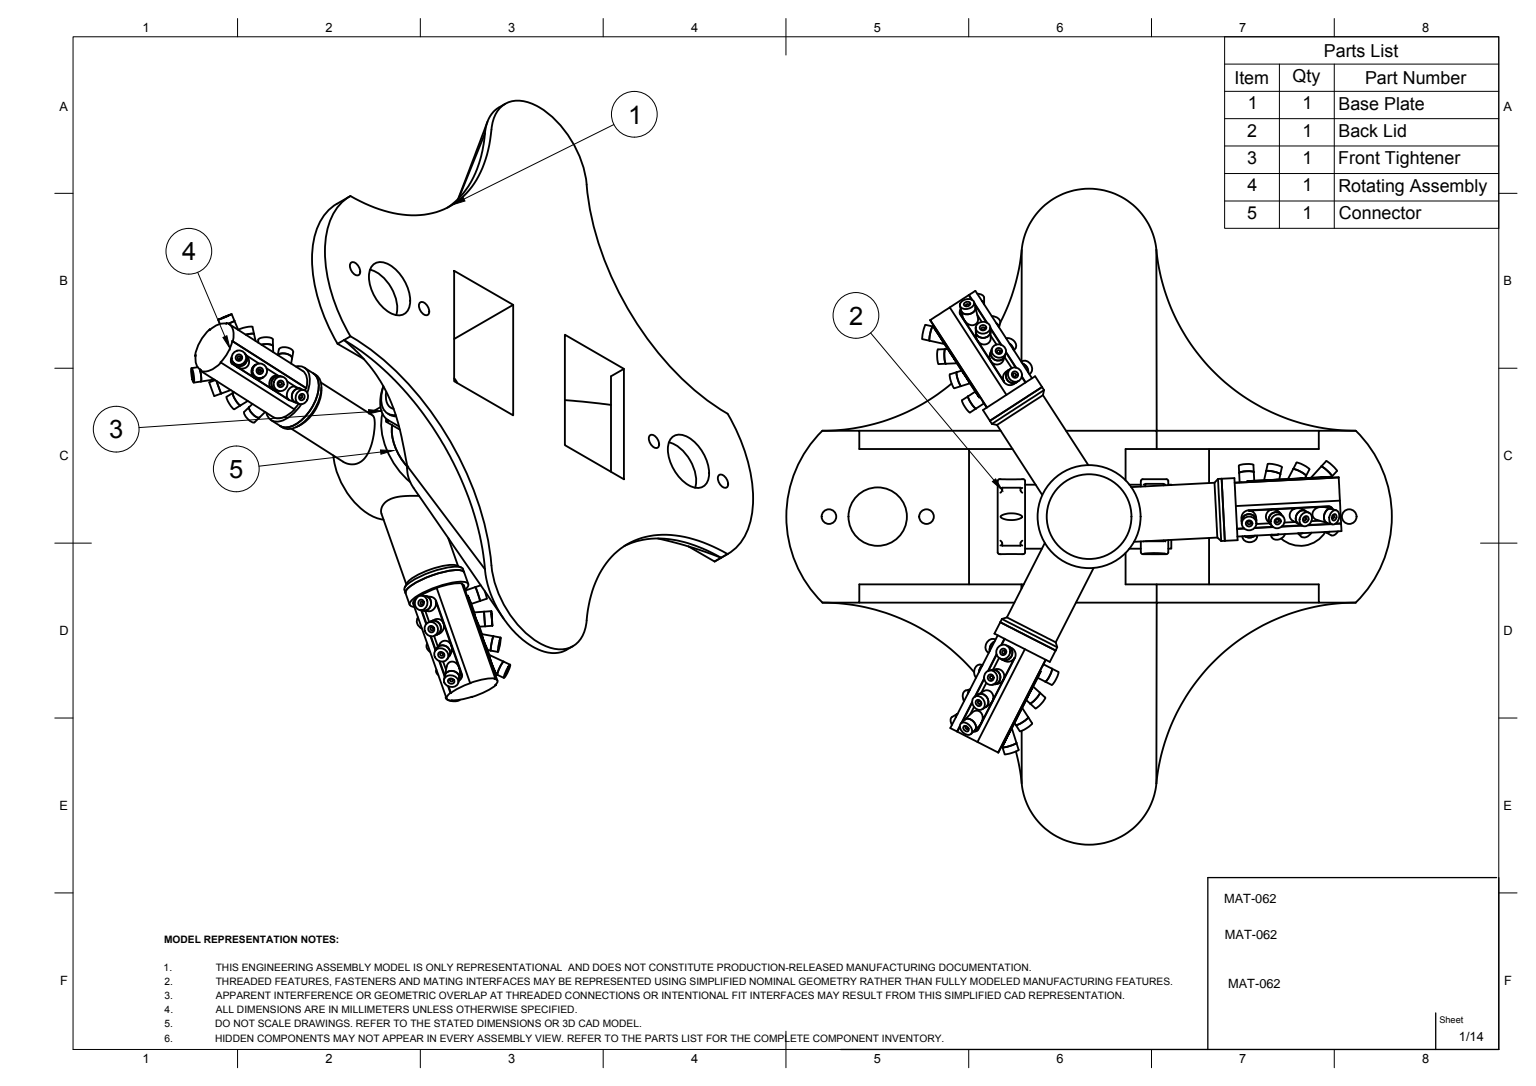
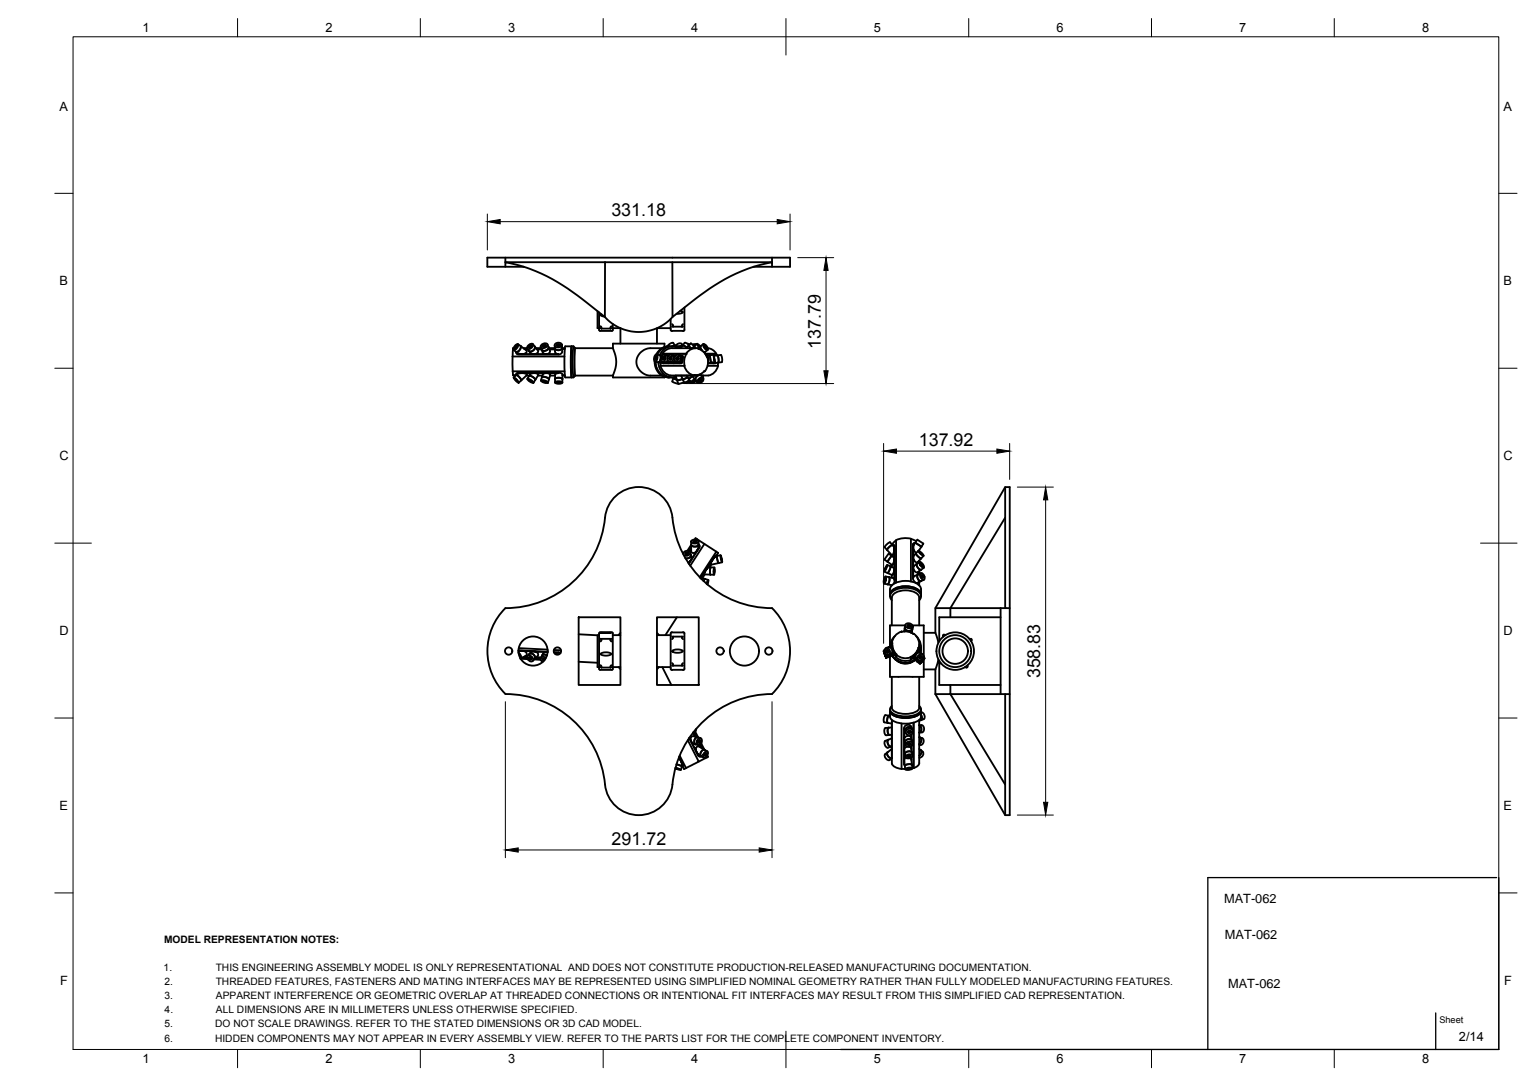
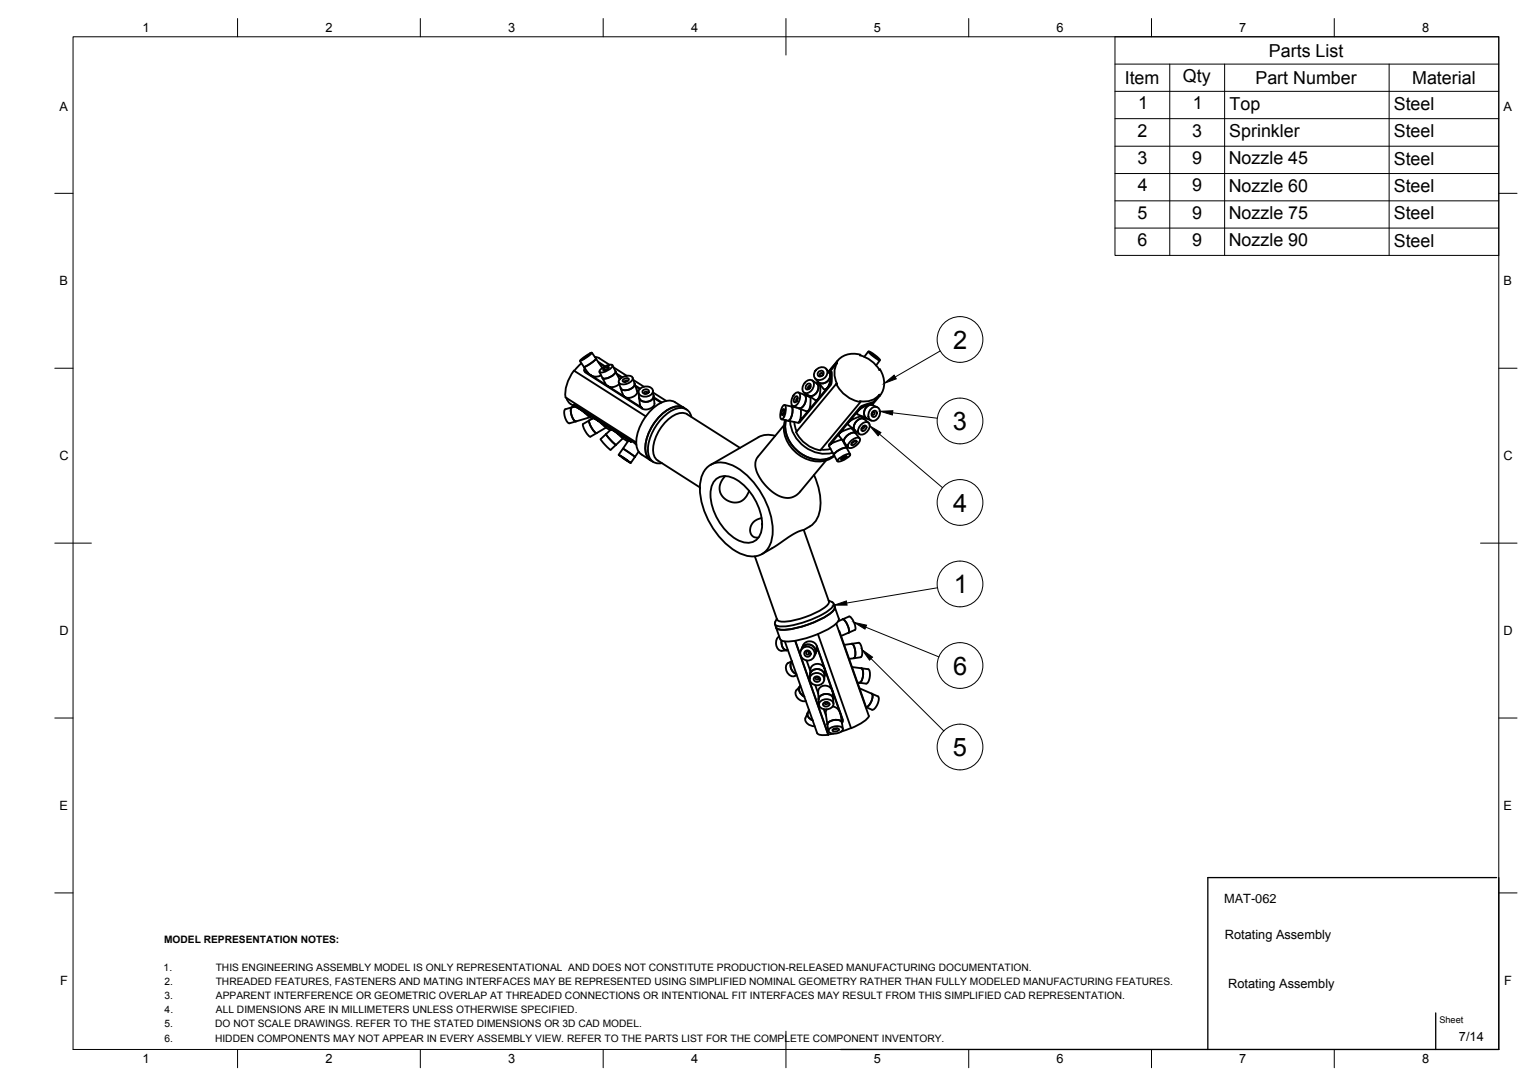
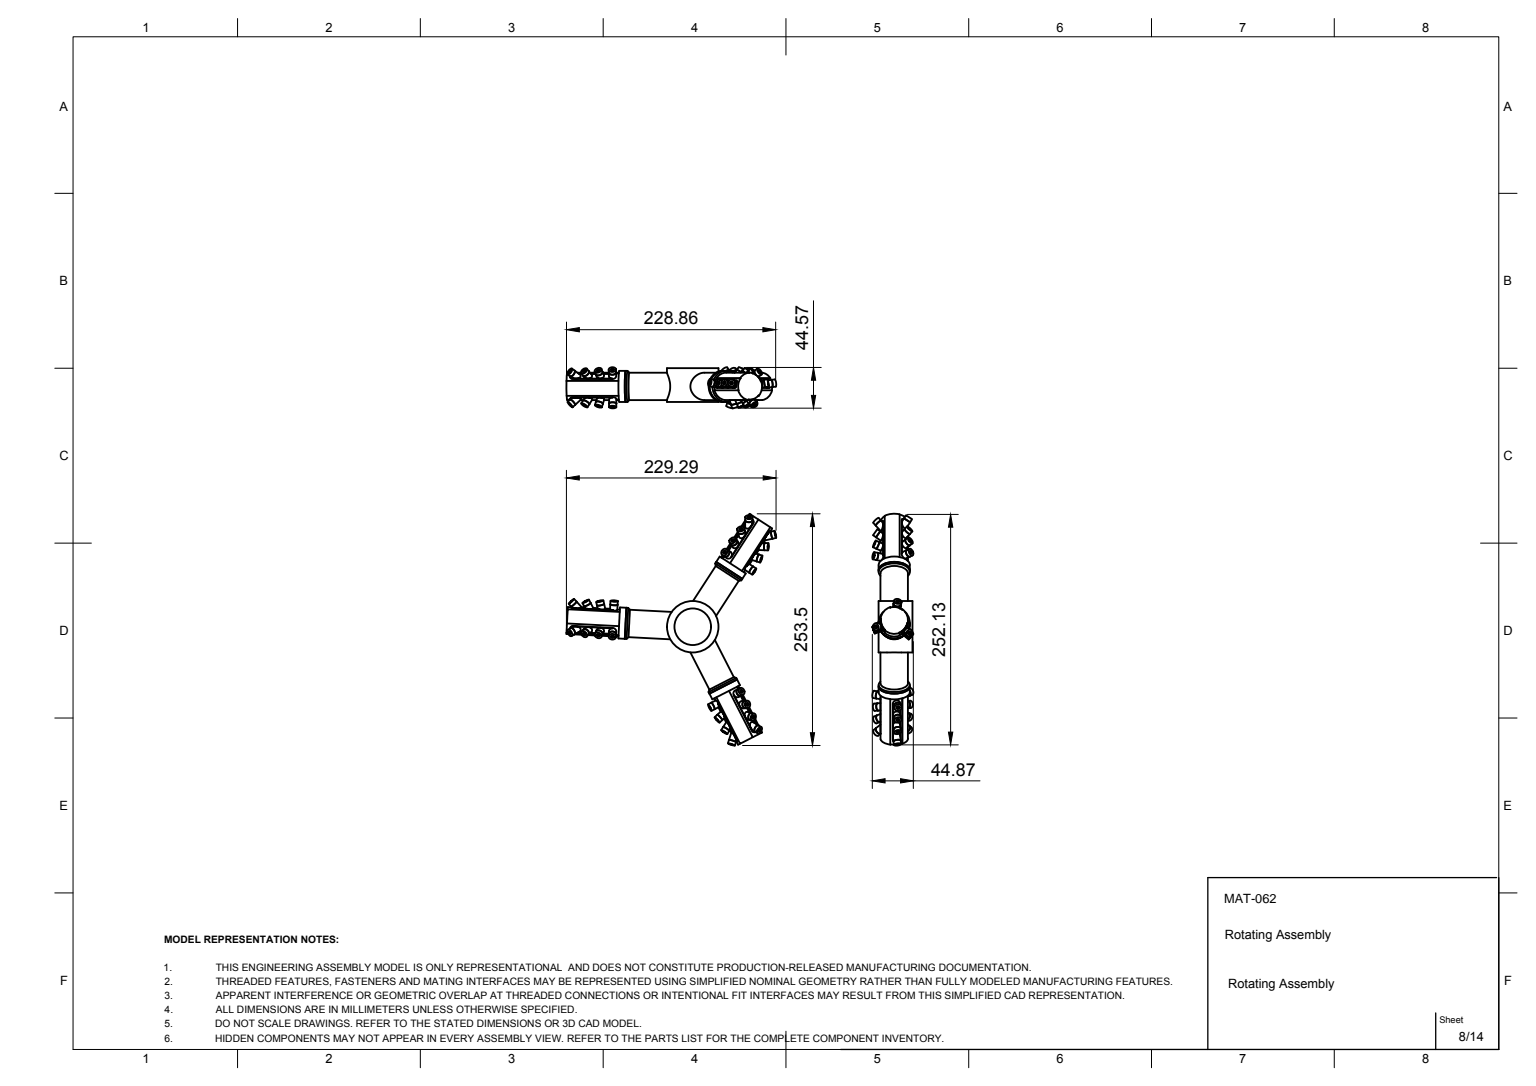
ISO-10303-21;
HEADER;
/* Generated by software containing ST-Developer
 * from STEP Tools, Inc. (www.steptools.com) 
 */

FILE_DESCRIPTION(
/* description */ (''),
/* implementation_level */ '2;1');

FILE_NAME(
/* name */ 'MAT-062',
/* time_stamp */ '2026-10-24T10:18:25-07:00',
/* author */ (''),
/* organization */ (''),
/* preprocessor_version */ 'ST-DEVELOPER v20.2',
/* originating_system */ 'Autodesk Translation Framework v15.15.0.0',
/* authorisation */ '');

FILE_SCHEMA (('AUTOMOTIVE_DESIGN { 1 0 10303 214 3 1 1 }'));
ENDSEC;

DATA;
#10=MECHANICAL_DESIGN_GEOMETRIC_PRESENTATION_REPRESENTATION('',(#247,#248,
#249,#250,#251,#252,#253,#254,#255,#256,#257,#258,#259,#260,#261,#262,#263,
#264,#265),#14125);
#11=ITEM_DEFINED_TRANSFORMATION($,$,#6478,#6849);
#12=ITEM_DEFINED_TRANSFORMATION($,$,#6669,#6850);
#13=ITEM_DEFINED_TRANSFORMATION($,$,#6624,#6851);
#14=ITEM_DEFINED_TRANSFORMATION($,$,#6609,#6852);
#15=ITEM_DEFINED_TRANSFORMATION($,$,#6639,#6853);
#16=ITEM_DEFINED_TRANSFORMATION($,$,#6654,#6854);
#17=ITEM_DEFINED_TRANSFORMATION($,$,#6624,#6855);
#18=ITEM_DEFINED_TRANSFORMATION($,$,#6624,#6856);
#19=ITEM_DEFINED_TRANSFORMATION($,$,#6609,#6857);
#20=ITEM_DEFINED_TRANSFORMATION($,$,#6609,#6858);
#21=ITEM_DEFINED_TRANSFORMATION($,$,#6639,#6859);
#22=ITEM_DEFINED_TRANSFORMATION($,$,#6639,#6860);
#23=ITEM_DEFINED_TRANSFORMATION($,$,#6654,#6861);
#24=ITEM_DEFINED_TRANSFORMATION($,$,#6654,#6862);
#25=ITEM_DEFINED_TRANSFORMATION($,$,#6654,#6863);
#26=ITEM_DEFINED_TRANSFORMATION($,$,#6654,#6864);
#27=ITEM_DEFINED_TRANSFORMATION($,$,#6639,#6865);
#28=ITEM_DEFINED_TRANSFORMATION($,$,#6639,#6866);
#29=ITEM_DEFINED_TRANSFORMATION($,$,#6609,#6867);
#30=ITEM_DEFINED_TRANSFORMATION($,$,#6609,#6868);
#31=ITEM_DEFINED_TRANSFORMATION($,$,#6624,#6869);
#32=ITEM_DEFINED_TRANSFORMATION($,$,#6624,#6870);
#33=ITEM_DEFINED_TRANSFORMATION($,$,#6609,#6871);
#34=ITEM_DEFINED_TRANSFORMATION($,$,#6609,#6872);
#35=ITEM_DEFINED_TRANSFORMATION($,$,#6624,#6873);
#36=ITEM_DEFINED_TRANSFORMATION($,$,#6624,#6874);
#37=ITEM_DEFINED_TRANSFORMATION($,$,#6639,#6875);
#38=ITEM_DEFINED_TRANSFORMATION($,$,#6639,#6876);
#39=ITEM_DEFINED_TRANSFORMATION($,$,#6654,#6877);
#40=ITEM_DEFINED_TRANSFORMATION($,$,#6654,#6878);
#41=ITEM_DEFINED_TRANSFORMATION($,$,#6609,#6879);
#42=ITEM_DEFINED_TRANSFORMATION($,$,#6609,#6880);
#43=ITEM_DEFINED_TRANSFORMATION($,$,#6624,#6881);
#44=ITEM_DEFINED_TRANSFORMATION($,$,#6624,#6882);
#45=ITEM_DEFINED_TRANSFORMATION($,$,#6639,#6883);
#46=ITEM_DEFINED_TRANSFORMATION($,$,#6639,#6884);
#47=ITEM_DEFINED_TRANSFORMATION($,$,#6654,#6885);
#48=ITEM_DEFINED_TRANSFORMATION($,$,#6654,#6886);
#49=ITEM_DEFINED_TRANSFORMATION($,$,#6669,#6887);
#50=ITEM_DEFINED_TRANSFORMATION($,$,#6669,#6888);
#51=ITEM_DEFINED_TRANSFORMATION($,$,#6259,#6902);
#52=ITEM_DEFINED_TRANSFORMATION($,$,#6338,#6903);
#53=ITEM_DEFINED_TRANSFORMATION($,$,#6408,#6904);
#54=ITEM_DEFINED_TRANSFORMATION($,$,#6477,#6905);
#55=ITEM_DEFINED_TRANSFORMATION($,$,#6889,#6906);
#56=(
REPRESENTATION_RELATIONSHIP($,$,#14204,#14203)
REPRESENTATION_RELATIONSHIP_WITH_TRANSFORMATION(#11)
SHAPE_REPRESENTATION_RELATIONSHIP()
);
#57=(
REPRESENTATION_RELATIONSHIP($,$,#14209,#14203)
REPRESENTATION_RELATIONSHIP_WITH_TRANSFORMATION(#12)
SHAPE_REPRESENTATION_RELATIONSHIP()
);
#58=(
REPRESENTATION_RELATIONSHIP($,$,#14206,#14203)
REPRESENTATION_RELATIONSHIP_WITH_TRANSFORMATION(#13)
SHAPE_REPRESENTATION_RELATIONSHIP()
);
#59=(
REPRESENTATION_RELATIONSHIP($,$,#14205,#14203)
REPRESENTATION_RELATIONSHIP_WITH_TRANSFORMATION(#14)
SHAPE_REPRESENTATION_RELATIONSHIP()
);
#60=(
REPRESENTATION_RELATIONSHIP($,$,#14207,#14203)
REPRESENTATION_RELATIONSHIP_WITH_TRANSFORMATION(#15)
SHAPE_REPRESENTATION_RELATIONSHIP()
);
#61=(
REPRESENTATION_RELATIONSHIP($,$,#14208,#14203)
REPRESENTATION_RELATIONSHIP_WITH_TRANSFORMATION(#16)
SHAPE_REPRESENTATION_RELATIONSHIP()
);
#62=(
REPRESENTATION_RELATIONSHIP($,$,#14206,#14203)
REPRESENTATION_RELATIONSHIP_WITH_TRANSFORMATION(#17)
SHAPE_REPRESENTATION_RELATIONSHIP()
);
#63=(
REPRESENTATION_RELATIONSHIP($,$,#14206,#14203)
REPRESENTATION_RELATIONSHIP_WITH_TRANSFORMATION(#18)
SHAPE_REPRESENTATION_RELATIONSHIP()
);
#64=(
REPRESENTATION_RELATIONSHIP($,$,#14205,#14203)
REPRESENTATION_RELATIONSHIP_WITH_TRANSFORMATION(#19)
SHAPE_REPRESENTATION_RELATIONSHIP()
);
#65=(
REPRESENTATION_RELATIONSHIP($,$,#14205,#14203)
REPRESENTATION_RELATIONSHIP_WITH_TRANSFORMATION(#20)
SHAPE_REPRESENTATION_RELATIONSHIP()
);
#66=(
REPRESENTATION_RELATIONSHIP($,$,#14207,#14203)
REPRESENTATION_RELATIONSHIP_WITH_TRANSFORMATION(#21)
SHAPE_REPRESENTATION_RELATIONSHIP()
);
#67=(
REPRESENTATION_RELATIONSHIP($,$,#14207,#14203)
REPRESENTATION_RELATIONSHIP_WITH_TRANSFORMATION(#22)
SHAPE_REPRESENTATION_RELATIONSHIP()
);
#68=(
REPRESENTATION_RELATIONSHIP($,$,#14208,#14203)
REPRESENTATION_RELATIONSHIP_WITH_TRANSFORMATION(#23)
SHAPE_REPRESENTATION_RELATIONSHIP()
);
#69=(
REPRESENTATION_RELATIONSHIP($,$,#14208,#14203)
REPRESENTATION_RELATIONSHIP_WITH_TRANSFORMATION(#24)
SHAPE_REPRESENTATION_RELATIONSHIP()
);
#70=(
REPRESENTATION_RELATIONSHIP($,$,#14208,#14203)
REPRESENTATION_RELATIONSHIP_WITH_TRANSFORMATION(#25)
SHAPE_REPRESENTATION_RELATIONSHIP()
);
#71=(
REPRESENTATION_RELATIONSHIP($,$,#14208,#14203)
REPRESENTATION_RELATIONSHIP_WITH_TRANSFORMATION(#26)
SHAPE_REPRESENTATION_RELATIONSHIP()
);
#72=(
REPRESENTATION_RELATIONSHIP($,$,#14207,#14203)
REPRESENTATION_RELATIONSHIP_WITH_TRANSFORMATION(#27)
SHAPE_REPRESENTATION_RELATIONSHIP()
);
#73=(
REPRESENTATION_RELATIONSHIP($,$,#14207,#14203)
REPRESENTATION_RELATIONSHIP_WITH_TRANSFORMATION(#28)
SHAPE_REPRESENTATION_RELATIONSHIP()
);
#74=(
REPRESENTATION_RELATIONSHIP($,$,#14205,#14203)
REPRESENTATION_RELATIONSHIP_WITH_TRANSFORMATION(#29)
SHAPE_REPRESENTATION_RELATIONSHIP()
);
#75=(
REPRESENTATION_RELATIONSHIP($,$,#14205,#14203)
REPRESENTATION_RELATIONSHIP_WITH_TRANSFORMATION(#30)
SHAPE_REPRESENTATION_RELATIONSHIP()
);
#76=(
REPRESENTATION_RELATIONSHIP($,$,#14206,#14203)
REPRESENTATION_RELATIONSHIP_WITH_TRANSFORMATION(#31)
SHAPE_REPRESENTATION_RELATIONSHIP()
);
#77=(
REPRESENTATION_RELATIONSHIP($,$,#14206,#14203)
REPRESENTATION_RELATIONSHIP_WITH_TRANSFORMATION(#32)
SHAPE_REPRESENTATION_RELATIONSHIP()
);
#78=(
REPRESENTATION_RELATIONSHIP($,$,#14205,#14203)
REPRESENTATION_RELATIONSHIP_WITH_TRANSFORMATION(#33)
SHAPE_REPRESENTATION_RELATIONSHIP()
);
#79=(
REPRESENTATION_RELATIONSHIP($,$,#14205,#14203)
REPRESENTATION_RELATIONSHIP_WITH_TRANSFORMATION(#34)
SHAPE_REPRESENTATION_RELATIONSHIP()
);
#80=(
REPRESENTATION_RELATIONSHIP($,$,#14206,#14203)
REPRESENTATION_RELATIONSHIP_WITH_TRANSFORMATION(#35)
SHAPE_REPRESENTATION_RELATIONSHIP()
);
#81=(
REPRESENTATION_RELATIONSHIP($,$,#14206,#14203)
REPRESENTATION_RELATIONSHIP_WITH_TRANSFORMATION(#36)
SHAPE_REPRESENTATION_RELATIONSHIP()
);
#82=(
REPRESENTATION_RELATIONSHIP($,$,#14207,#14203)
REPRESENTATION_RELATIONSHIP_WITH_TRANSFORMATION(#37)
SHAPE_REPRESENTATION_RELATIONSHIP()
);
#83=(
REPRESENTATION_RELATIONSHIP($,$,#14207,#14203)
REPRESENTATION_RELATIONSHIP_WITH_TRANSFORMATION(#38)
SHAPE_REPRESENTATION_RELATIONSHIP()
);
#84=(
REPRESENTATION_RELATIONSHIP($,$,#14208,#14203)
REPRESENTATION_RELATIONSHIP_WITH_TRANSFORMATION(#39)
SHAPE_REPRESENTATION_RELATIONSHIP()
);
#85=(
REPRESENTATION_RELATIONSHIP($,$,#14208,#14203)
REPRESENTATION_RELATIONSHIP_WITH_TRANSFORMATION(#40)
SHAPE_REPRESENTATION_RELATIONSHIP()
);
#86=(
REPRESENTATION_RELATIONSHIP($,$,#14205,#14203)
REPRESENTATION_RELATIONSHIP_WITH_TRANSFORMATION(#41)
SHAPE_REPRESENTATION_RELATIONSHIP()
);
#87=(
REPRESENTATION_RELATIONSHIP($,$,#14205,#14203)
REPRESENTATION_RELATIONSHIP_WITH_TRANSFORMATION(#42)
SHAPE_REPRESENTATION_RELATIONSHIP()
);
#88=(
REPRESENTATION_RELATIONSHIP($,$,#14206,#14203)
REPRESENTATION_RELATIONSHIP_WITH_TRANSFORMATION(#43)
SHAPE_REPRESENTATION_RELATIONSHIP()
);
#89=(
REPRESENTATION_RELATIONSHIP($,$,#14206,#14203)
REPRESENTATION_RELATIONSHIP_WITH_TRANSFORMATION(#44)
SHAPE_REPRESENTATION_RELATIONSHIP()
);
#90=(
REPRESENTATION_RELATIONSHIP($,$,#14207,#14203)
REPRESENTATION_RELATIONSHIP_WITH_TRANSFORMATION(#45)
SHAPE_REPRESENTATION_RELATIONSHIP()
);
#91=(
REPRESENTATION_RELATIONSHIP($,$,#14207,#14203)
REPRESENTATION_RELATIONSHIP_WITH_TRANSFORMATION(#46)
SHAPE_REPRESENTATION_RELATIONSHIP()
);
#92=(
REPRESENTATION_RELATIONSHIP($,$,#14208,#14203)
REPRESENTATION_RELATIONSHIP_WITH_TRANSFORMATION(#47)
SHAPE_REPRESENTATION_RELATIONSHIP()
);
#93=(
REPRESENTATION_RELATIONSHIP($,$,#14208,#14203)
REPRESENTATION_RELATIONSHIP_WITH_TRANSFORMATION(#48)
SHAPE_REPRESENTATION_RELATIONSHIP()
);
#94=(
REPRESENTATION_RELATIONSHIP($,$,#14209,#14203)
REPRESENTATION_RELATIONSHIP_WITH_TRANSFORMATION(#49)
SHAPE_REPRESENTATION_RELATIONSHIP()
);
#95=(
REPRESENTATION_RELATIONSHIP($,$,#14209,#14203)
REPRESENTATION_RELATIONSHIP_WITH_TRANSFORMATION(#50)
SHAPE_REPRESENTATION_RELATIONSHIP()
);
#96=(
REPRESENTATION_RELATIONSHIP($,$,#14200,#14199)
REPRESENTATION_RELATIONSHIP_WITH_TRANSFORMATION(#51)
SHAPE_REPRESENTATION_RELATIONSHIP()
);
#97=(
REPRESENTATION_RELATIONSHIP($,$,#14201,#14199)
REPRESENTATION_RELATIONSHIP_WITH_TRANSFORMATION(#52)
SHAPE_REPRESENTATION_RELATIONSHIP()
);
#98=(
REPRESENTATION_RELATIONSHIP($,$,#14202,#14199)
REPRESENTATION_RELATIONSHIP_WITH_TRANSFORMATION(#53)
SHAPE_REPRESENTATION_RELATIONSHIP()
);
#99=(
REPRESENTATION_RELATIONSHIP($,$,#14203,#14199)
REPRESENTATION_RELATIONSHIP_WITH_TRANSFORMATION(#54)
SHAPE_REPRESENTATION_RELATIONSHIP()
);
#100=(
REPRESENTATION_RELATIONSHIP($,$,#14210,#14199)
REPRESENTATION_RELATIONSHIP_WITH_TRANSFORMATION(#55)
SHAPE_REPRESENTATION_RELATIONSHIP()
);
#101=CONTEXT_DEPENDENT_SHAPE_REPRESENTATION(#56,#14153);
#102=CONTEXT_DEPENDENT_SHAPE_REPRESENTATION(#57,#14154);
#103=CONTEXT_DEPENDENT_SHAPE_REPRESENTATION(#58,#14155);
#104=CONTEXT_DEPENDENT_SHAPE_REPRESENTATION(#59,#14156);
#105=CONTEXT_DEPENDENT_SHAPE_REPRESENTATION(#60,#14157);
#106=CONTEXT_DEPENDENT_SHAPE_REPRESENTATION(#61,#14158);
#107=CONTEXT_DEPENDENT_SHAPE_REPRESENTATION(#62,#14159);
#108=CONTEXT_DEPENDENT_SHAPE_REPRESENTATION(#63,#14160);
#109=CONTEXT_DEPENDENT_SHAPE_REPRESENTATION(#64,#14161);
#110=CONTEXT_DEPENDENT_SHAPE_REPRESENTATION(#65,#14162);
#111=CONTEXT_DEPENDENT_SHAPE_REPRESENTATION(#66,#14163);
#112=CONTEXT_DEPENDENT_SHAPE_REPRESENTATION(#67,#14164);
#113=CONTEXT_DEPENDENT_SHAPE_REPRESENTATION(#68,#14165);
#114=CONTEXT_DEPENDENT_SHAPE_REPRESENTATION(#69,#14166);
#115=CONTEXT_DEPENDENT_SHAPE_REPRESENTATION(#70,#14167);
#116=CONTEXT_DEPENDENT_SHAPE_REPRESENTATION(#71,#14168);
#117=CONTEXT_DEPENDENT_SHAPE_REPRESENTATION(#72,#14169);
#118=CONTEXT_DEPENDENT_SHAPE_REPRESENTATION(#73,#14170);
#119=CONTEXT_DEPENDENT_SHAPE_REPRESENTATION(#74,#14171);
#120=CONTEXT_DEPENDENT_SHAPE_REPRESENTATION(#75,#14172);
#121=CONTEXT_DEPENDENT_SHAPE_REPRESENTATION(#76,#14173);
#122=CONTEXT_DEPENDENT_SHAPE_REPRESENTATION(#77,#14174);
#123=CONTEXT_DEPENDENT_SHAPE_REPRESENTATION(#78,#14175);
#124=CONTEXT_DEPENDENT_SHAPE_REPRESENTATION(#79,#14176);
#125=CONTEXT_DEPENDENT_SHAPE_REPRESENTATION(#80,#14177);
#126=CONTEXT_DEPENDENT_SHAPE_REPRESENTATION(#81,#14178);
#127=CONTEXT_DEPENDENT_SHAPE_REPRESENTATION(#82,#14179);
#128=CONTEXT_DEPENDENT_SHAPE_REPRESENTATION(#83,#14180);
#129=CONTEXT_DEPENDENT_SHAPE_REPRESENTATION(#84,#14181);
#130=CONTEXT_DEPENDENT_SHAPE_REPRESENTATION(#85,#14182);
#131=CONTEXT_DEPENDENT_SHAPE_REPRESENTATION(#86,#14183);
#132=CONTEXT_DEPENDENT_SHAPE_REPRESENTATION(#87,#14184);
#133=CONTEXT_DEPENDENT_SHAPE_REPRESENTATION(#88,#14185);
#134=CONTEXT_DEPENDENT_SHAPE_REPRESENTATION(#89,#14186);
#135=CONTEXT_DEPENDENT_SHAPE_REPRESENTATION(#90,#14187);
#136=CONTEXT_DEPENDENT_SHAPE_REPRESENTATION(#91,#14188);
#137=CONTEXT_DEPENDENT_SHAPE_REPRESENTATION(#92,#14189);
#138=CONTEXT_DEPENDENT_SHAPE_REPRESENTATION(#93,#14190);
#139=CONTEXT_DEPENDENT_SHAPE_REPRESENTATION(#94,#14191);
#140=CONTEXT_DEPENDENT_SHAPE_REPRESENTATION(#95,#14192);
#141=CONTEXT_DEPENDENT_SHAPE_REPRESENTATION(#96,#14194);
#142=CONTEXT_DEPENDENT_SHAPE_REPRESENTATION(#97,#14195);
#143=CONTEXT_DEPENDENT_SHAPE_REPRESENTATION(#98,#14196);
#144=CONTEXT_DEPENDENT_SHAPE_REPRESENTATION(#99,#14197);
#145=CONTEXT_DEPENDENT_SHAPE_REPRESENTATION(#100,#14198);
#146=NEXT_ASSEMBLY_USAGE_OCCURRENCE('Top:1','Top:1','Top:1',#14216,#14217,
'Top:1');
#147=NEXT_ASSEMBLY_USAGE_OCCURRENCE('Sprinkler:1','Sprinkler:1',
'Sprinkler:1',#14216,#14222,'Sprinkler:1');
#148=NEXT_ASSEMBLY_USAGE_OCCURRENCE('Nozzle 45:1','Nozzle 45:1',
'Nozzle 45:1',#14216,#14219,'Nozzle 45:1');
#149=NEXT_ASSEMBLY_USAGE_OCCURRENCE('Nozzle 60:1','Nozzle 60:1',
'Nozzle 60:1',#14216,#14218,'Nozzle 60:1');
#150=NEXT_ASSEMBLY_USAGE_OCCURRENCE('Nozzle 75:1','Nozzle 75:1',
'Nozzle 75:1',#14216,#14220,'Nozzle 75:1');
#151=NEXT_ASSEMBLY_USAGE_OCCURRENCE('Nozzle 90:1','Nozzle 90:1',
'Nozzle 90:1',#14216,#14221,'Nozzle 90:1');
#152=NEXT_ASSEMBLY_USAGE_OCCURRENCE('Nozzle 45:2','Nozzle 45:2',
'Nozzle 45:2',#14216,#14219,'Nozzle 45:2');
#153=NEXT_ASSEMBLY_USAGE_OCCURRENCE('Nozzle 45:3','Nozzle 45:3',
'Nozzle 45:3',#14216,#14219,'Nozzle 45:3');
#154=NEXT_ASSEMBLY_USAGE_OCCURRENCE('Nozzle 60:2','Nozzle 60:2',
'Nozzle 60:2',#14216,#14218,'Nozzle 60:2');
#155=NEXT_ASSEMBLY_USAGE_OCCURRENCE('Nozzle 60:3','Nozzle 60:3',
'Nozzle 60:3',#14216,#14218,'Nozzle 60:3');
#156=NEXT_ASSEMBLY_USAGE_OCCURRENCE('Nozzle 75:2','Nozzle 75:2',
'Nozzle 75:2',#14216,#14220,'Nozzle 75:2');
#157=NEXT_ASSEMBLY_USAGE_OCCURRENCE('Nozzle 75:3','Nozzle 75:3',
'Nozzle 75:3',#14216,#14220,'Nozzle 75:3');
#158=NEXT_ASSEMBLY_USAGE_OCCURRENCE('Nozzle 90:2','Nozzle 90:2',
'Nozzle 90:2',#14216,#14221,'Nozzle 90:2');
#159=NEXT_ASSEMBLY_USAGE_OCCURRENCE('Nozzle 90:3','Nozzle 90:3',
'Nozzle 90:3',#14216,#14221,'Nozzle 90:3');
#160=NEXT_ASSEMBLY_USAGE_OCCURRENCE('Nozzle 90:4','Nozzle 90:4',
'Nozzle 90:4',#14216,#14221,'Nozzle 90:4');
#161=NEXT_ASSEMBLY_USAGE_OCCURRENCE('Nozzle 90:5','Nozzle 90:5',
'Nozzle 90:5',#14216,#14221,'Nozzle 90:5');
#162=NEXT_ASSEMBLY_USAGE_OCCURRENCE('Nozzle 75:4','Nozzle 75:4',
'Nozzle 75:4',#14216,#14220,'Nozzle 75:4');
#163=NEXT_ASSEMBLY_USAGE_OCCURRENCE('Nozzle 75:5','Nozzle 75:5',
'Nozzle 75:5',#14216,#14220,'Nozzle 75:5');
#164=NEXT_ASSEMBLY_USAGE_OCCURRENCE('Nozzle 60:4','Nozzle 60:4',
'Nozzle 60:4',#14216,#14218,'Nozzle 60:4');
#165=NEXT_ASSEMBLY_USAGE_OCCURRENCE('Nozzle 60:5','Nozzle 60:5',
'Nozzle 60:5',#14216,#14218,'Nozzle 60:5');
#166=NEXT_ASSEMBLY_USAGE_OCCURRENCE('Nozzle 45:4','Nozzle 45:4',
'Nozzle 45:4',#14216,#14219,'Nozzle 45:4');
#167=NEXT_ASSEMBLY_USAGE_OCCURRENCE('Nozzle 45:5','Nozzle 45:5',
'Nozzle 45:5',#14216,#14219,'Nozzle 45:5');
#168=NEXT_ASSEMBLY_USAGE_OCCURRENCE('Nozzle 60:6','Nozzle 60:6',
'Nozzle 60:6',#14216,#14218,'Nozzle 60:6');
#169=NEXT_ASSEMBLY_USAGE_OCCURRENCE('Nozzle 60:7','Nozzle 60:7',
'Nozzle 60:7',#14216,#14218,'Nozzle 60:7');
#170=NEXT_ASSEMBLY_USAGE_OCCURRENCE('Nozzle 45:6','Nozzle 45:6',
'Nozzle 45:6',#14216,#14219,'Nozzle 45:6');
#171=NEXT_ASSEMBLY_USAGE_OCCURRENCE('Nozzle 45:7','Nozzle 45:7',
'Nozzle 45:7',#14216,#14219,'Nozzle 45:7');
#172=NEXT_ASSEMBLY_USAGE_OCCURRENCE('Nozzle 75:6','Nozzle 75:6',
'Nozzle 75:6',#14216,#14220,'Nozzle 75:6');
#173=NEXT_ASSEMBLY_USAGE_OCCURRENCE('Nozzle 75:7','Nozzle 75:7',
'Nozzle 75:7',#14216,#14220,'Nozzle 75:7');
#174=NEXT_ASSEMBLY_USAGE_OCCURRENCE('Nozzle 90:6','Nozzle 90:6',
'Nozzle 90:6',#14216,#14221,'Nozzle 90:6');
#175=NEXT_ASSEMBLY_USAGE_OCCURRENCE('Nozzle 90:7','Nozzle 90:7',
'Nozzle 90:7',#14216,#14221,'Nozzle 90:7');
#176=NEXT_ASSEMBLY_USAGE_OCCURRENCE('Nozzle 60:8','Nozzle 60:8',
'Nozzle 60:8',#14216,#14218,'Nozzle 60:8');
#177=NEXT_ASSEMBLY_USAGE_OCCURRENCE('Nozzle 60:9','Nozzle 60:9',
'Nozzle 60:9',#14216,#14218,'Nozzle 60:9');
#178=NEXT_ASSEMBLY_USAGE_OCCURRENCE('Nozzle 45:8','Nozzle 45:8',
'Nozzle 45:8',#14216,#14219,'Nozzle 45:8');
#179=NEXT_ASSEMBLY_USAGE_OCCURRENCE('Nozzle 45:9','Nozzle 45:9',
'Nozzle 45:9',#14216,#14219,'Nozzle 45:9');
#180=NEXT_ASSEMBLY_USAGE_OCCURRENCE('Nozzle 75:8','Nozzle 75:8',
'Nozzle 75:8',#14216,#14220,'Nozzle 75:8');
#181=NEXT_ASSEMBLY_USAGE_OCCURRENCE('Nozzle 75:9','Nozzle 75:9',
'Nozzle 75:9',#14216,#14220,'Nozzle 75:9');
#182=NEXT_ASSEMBLY_USAGE_OCCURRENCE('Nozzle 90:8','Nozzle 90:8',
'Nozzle 90:8',#14216,#14221,'Nozzle 90:8');
#183=NEXT_ASSEMBLY_USAGE_OCCURRENCE('Nozzle 90:9','Nozzle 90:9',
'Nozzle 90:9',#14216,#14221,'Nozzle 90:9');
#184=NEXT_ASSEMBLY_USAGE_OCCURRENCE('Sprinkler:2','Sprinkler:2',
'Sprinkler:2',#14216,#14222,'Sprinkler:2');
#185=NEXT_ASSEMBLY_USAGE_OCCURRENCE('Sprinkler:3','Sprinkler:3',
'Sprinkler:3',#14216,#14222,'Sprinkler:3');
#186=NEXT_ASSEMBLY_USAGE_OCCURRENCE('Base Plate:1','Base Plate:1',
'Base Plate:1',#14212,#14213,'Base Plate:1');
#187=NEXT_ASSEMBLY_USAGE_OCCURRENCE('Back Lid:1','Back Lid:1',
'Back Lid:1',#14212,#14214,'Back Lid:1');
#188=NEXT_ASSEMBLY_USAGE_OCCURRENCE('Front Tightener:1',
'Front Tightener:1','Front Tightener:1',#14212,#14215,
'Front Tightener:1');
#189=NEXT_ASSEMBLY_USAGE_OCCURRENCE('Rotating Assembly:1',
'Rotating Assembly:1','Rotating Assembly:1',#14212,#14216,
'Rotating Assembly:1');
#190=NEXT_ASSEMBLY_USAGE_OCCURRENCE('Connector:1','Connector:1',
'Connector:1',#14212,#14223,'Connector:1');
#191=CONICAL_SURFACE('',#6560,17.,0.785398163397448);
#192=CONICAL_SURFACE('',#6577,17.,0.785398163397452);
#193=CONICAL_SURFACE('',#6578,17.,0.785398163397448);
#194=CONICAL_SURFACE('',#6620,1.8,0.785398163397439);
#195=CONICAL_SURFACE('',#6635,1.8,0.785398163397447);
#196=CONICAL_SURFACE('',#6650,1.80000000000001,0.785398163397454);
#197=CONICAL_SURFACE('',#6665,1.8,0.785398163397448);
#198=CONICAL_SURFACE('',#6890,16.,0.0349065850398866);
#199=TOROIDAL_SURFACE('',#6365,21.5,1.);
#200=TOROIDAL_SURFACE('',#6366,21.5,1.);
#201=TOROIDAL_SURFACE('',#6390,21.5,1.);
#202=TOROIDAL_SURFACE('',#6391,21.5,1.);
#203=TOROIDAL_SURFACE('',#6394,21.5,1.);
#204=TOROIDAL_SURFACE('',#6395,21.5,1.);
#205=TOROIDAL_SURFACE('',#6398,21.5,1.);
#206=TOROIDAL_SURFACE('',#6399,21.5,1.);
#207=TOROIDAL_SURFACE('',#6401,19.5,1.);
#208=TOROIDAL_SURFACE('',#6403,19.5,1.);
#209=TOROIDAL_SURFACE('',#6436,21.5,1.);
#210=TOROIDAL_SURFACE('',#6437,21.5,1.);
#211=TOROIDAL_SURFACE('',#6461,21.5,1.);
#212=TOROIDAL_SURFACE('',#6462,21.5,1.);
#213=TOROIDAL_SURFACE('',#6465,21.5,1.);
#214=TOROIDAL_SURFACE('',#6466,21.5,1.);
#215=TOROIDAL_SURFACE('',#6469,21.5,1.);
#216=TOROIDAL_SURFACE('',#6470,21.5,1.);
#217=TOROIDAL_SURFACE('',#6472,19.5,1.);
#218=TOROIDAL_SURFACE('',#6474,19.5,1.);
#219=(
BOUNDED_SURFACE()
B_SPLINE_SURFACE(2,2,((#10435,#10436,#10437,#10438,#10439),(#10440,#10441,
#10442,#10443,#10444),(#10445,#10446,#10447,#10448,#10449)),
 .UNSPECIFIED.,.F.,.F.,.F.)
B_SPLINE_SURFACE_WITH_KNOTS((3,3),(3,2,3),(-0.372145961557786,0.372122372471418),
(-2.5862005619648,-1.57539112175776,-0.564581681550713),.UNSPECIFIED.)
GEOMETRIC_REPRESENTATION_ITEM()
RATIONAL_B_SPLINE_SURFACE(((1.,0.874978596158143,1.,0.874978596158143,1.),
(0.931553475244656,0.815089352015808,0.931553475244656,0.815089352015808,
0.931553475244656),(1.,0.874978596158143,1.,0.874978596158143,1.)))
REPRESENTATION_ITEM('')
SURFACE()
);
#220=(
BOUNDED_SURFACE()
B_SPLINE_SURFACE(2,2,((#10450,#10451,#10452,#10453,#10454),(#10455,#10456,
#10457,#10458,#10459),(#10460,#10461,#10462,#10463,#10464)),
 .UNSPECIFIED.,.F.,.F.,.F.)
B_SPLINE_SURFACE_WITH_KNOTS((3,3),(3,2,3),(-0.372145961557785,0.372122372471416),
(-1.01540423516984,-0.00459479496282911,1.00621464524418),.UNSPECIFIED.)
GEOMETRIC_REPRESENTATION_ITEM()
RATIONAL_B_SPLINE_SURFACE(((1.,0.874978596158151,1.,0.874978596158151,1.),
(0.931553475244656,0.815089352015816,0.931553475244656,0.815089352015816,
0.931553475244656),(1.,0.874978596158151,1.,0.874978596158151,1.)))
REPRESENTATION_ITEM('')
SURFACE()
);
#221=(
BOUNDED_SURFACE()
B_SPLINE_SURFACE(2,2,((#10465,#10466,#10467,#10468,#10469),(#10470,#10471,
#10472,#10473,#10474),(#10475,#10476,#10477,#10478,#10479)),
 .UNSPECIFIED.,.F.,.F.,.F.)
B_SPLINE_SURFACE_WITH_KNOTS((3,3),(3,2,3),(-0.372145961557786,0.372122372471418),
(0.555392091624955,1.56620153183202,2.57701097203908),.UNSPECIFIED.)
GEOMETRIC_REPRESENTATION_ITEM()
RATIONAL_B_SPLINE_SURFACE(((1.,0.874978596158138,1.,0.874978596158138,1.),
(0.931553475244654,0.815089352015803,0.931553475244654,0.815089352015803,
0.931553475244654),(1.,0.874978596158138,1.,0.874978596158138,1.)))
REPRESENTATION_ITEM('')
SURFACE()
);
#222=(
BOUNDED_SURFACE()
B_SPLINE_SURFACE(2,2,((#10480,#10481,#10482,#10483,#10484),(#10485,#10486,
#10487,#10488,#10489),(#10490,#10491,#10492,#10493,#10494)),
 .UNSPECIFIED.,.F.,.F.,.F.)
B_SPLINE_SURFACE_WITH_KNOTS((3,3),(3,2,3),(-0.371934671474245,0.371934671474244),
(-1.01080944020701,0.,1.01080944020701),.UNSPECIFIED.)
GEOMETRIC_REPRESENTATION_ITEM()
RATIONAL_B_SPLINE_SURFACE(((1.,0.87497859615815,1.,0.87497859615815,1.),
(0.93162599415309,0.815152804508512,0.93162599415309,0.815152804508512,
0.93162599415309),(1.,0.87497859615815,1.,0.87497859615815,1.)))
REPRESENTATION_ITEM('')
SURFACE()
);
#223=(
BOUNDED_SURFACE()
B_SPLINE_SURFACE(2,2,((#11091,#11092,#11093,#11094,#11095),(#11096,#11097,
#11098,#11099,#11100),(#11101,#11102,#11103,#11104,#11105)),
 .UNSPECIFIED.,.F.,.F.,.F.)
B_SPLINE_SURFACE_WITH_KNOTS((3,3),(3,2,3),(-0.372145961557786,0.372122372471418),
(-2.5862005619648,-1.57539112175776,-0.564581681550713),.UNSPECIFIED.)
GEOMETRIC_REPRESENTATION_ITEM()
RATIONAL_B_SPLINE_SURFACE(((1.,0.874978596158143,1.,0.874978596158143,1.),
(0.931553475244656,0.815089352015808,0.931553475244656,0.815089352015808,
0.931553475244656),(1.,0.874978596158143,1.,0.874978596158143,1.)))
REPRESENTATION_ITEM('')
SURFACE()
);
#224=(
BOUNDED_SURFACE()
B_SPLINE_SURFACE(2,2,((#11106,#11107,#11108,#11109,#11110),(#11111,#11112,
#11113,#11114,#11115),(#11116,#11117,#11118,#11119,#11120)),
 .UNSPECIFIED.,.F.,.F.,.F.)
B_SPLINE_SURFACE_WITH_KNOTS((3,3),(3,2,3),(-0.372145961557785,0.372122372471416),
(-1.01540423516984,-0.00459479496282911,1.00621464524418),.UNSPECIFIED.)
GEOMETRIC_REPRESENTATION_ITEM()
RATIONAL_B_SPLINE_SURFACE(((1.,0.874978596158151,1.,0.874978596158151,1.),
(0.931553475244656,0.815089352015816,0.931553475244656,0.815089352015816,
0.931553475244656),(1.,0.874978596158151,1.,0.874978596158151,1.)))
REPRESENTATION_ITEM('')
SURFACE()
);
#225=(
BOUNDED_SURFACE()
B_SPLINE_SURFACE(2,2,((#11121,#11122,#11123,#11124,#11125),(#11126,#11127,
#11128,#11129,#11130),(#11131,#11132,#11133,#11134,#11135)),
 .UNSPECIFIED.,.F.,.F.,.F.)
B_SPLINE_SURFACE_WITH_KNOTS((3,3),(3,2,3),(-0.372145961557786,0.372122372471418),
(0.555392091624955,1.56620153183202,2.57701097203908),.UNSPECIFIED.)
GEOMETRIC_REPRESENTATION_ITEM()
RATIONAL_B_SPLINE_SURFACE(((1.,0.874978596158138,1.,0.874978596158138,1.),
(0.931553475244654,0.815089352015803,0.931553475244654,0.815089352015803,
0.931553475244654),(1.,0.874978596158138,1.,0.874978596158138,1.)))
REPRESENTATION_ITEM('')
SURFACE()
);
#226=(
BOUNDED_SURFACE()
B_SPLINE_SURFACE(2,2,((#11136,#11137,#11138,#11139,#11140),(#11141,#11142,
#11143,#11144,#11145),(#11146,#11147,#11148,#11149,#11150)),
 .UNSPECIFIED.,.F.,.F.,.F.)
B_SPLINE_SURFACE_WITH_KNOTS((3,3),(3,2,3),(-0.371934671474245,0.371934671474244),
(-1.01080944020701,0.,1.01080944020701),.UNSPECIFIED.)
GEOMETRIC_REPRESENTATION_ITEM()
RATIONAL_B_SPLINE_SURFACE(((1.,0.87497859615815,1.,0.87497859615815,1.),
(0.93162599415309,0.815152804508512,0.93162599415309,0.815152804508512,
0.93162599415309),(1.,0.87497859615815,1.,0.87497859615815,1.)))
REPRESENTATION_ITEM('')
SURFACE()
);
#227=SHAPE_REPRESENTATION_RELATIONSHIP('SRR','None',#14200,#237);
#228=SHAPE_REPRESENTATION_RELATIONSHIP('SRR','None',#14201,#238);
#229=SHAPE_REPRESENTATION_RELATIONSHIP('SRR','None',#14202,#239);
#230=SHAPE_REPRESENTATION_RELATIONSHIP('SRR','None',#14204,#240);
#231=SHAPE_REPRESENTATION_RELATIONSHIP('SRR','None',#14205,#241);
#232=SHAPE_REPRESENTATION_RELATIONSHIP('SRR','None',#14206,#242);
#233=SHAPE_REPRESENTATION_RELATIONSHIP('SRR','None',#14207,#243);
#234=SHAPE_REPRESENTATION_RELATIONSHIP('SRR','None',#14208,#244);
#235=SHAPE_REPRESENTATION_RELATIONSHIP('SRR','None',#14209,#245);
#236=SHAPE_REPRESENTATION_RELATIONSHIP('SRR','None',#14210,#246);
#237=ADVANCED_BREP_SHAPE_REPRESENTATION('',(#266),#14114);
#238=ADVANCED_BREP_SHAPE_REPRESENTATION('',(#267),#14115);
#239=ADVANCED_BREP_SHAPE_REPRESENTATION('',(#268),#14116);
#240=ADVANCED_BREP_SHAPE_REPRESENTATION('',(#269,#270,#271,#272),#14118);
#241=ADVANCED_BREP_SHAPE_REPRESENTATION('',(#273),#14119);
#242=ADVANCED_BREP_SHAPE_REPRESENTATION('',(#274),#14120);
#243=ADVANCED_BREP_SHAPE_REPRESENTATION('',(#275),#14121);
#244=ADVANCED_BREP_SHAPE_REPRESENTATION('',(#276),#14122);
#245=ADVANCED_BREP_SHAPE_REPRESENTATION('',(#277),#14123);
#246=ADVANCED_BREP_SHAPE_REPRESENTATION('',(#278),#14124);
#247=STYLED_ITEM('',(#14263),#266);
#248=STYLED_ITEM('',(#14263),#267);
#249=STYLED_ITEM('',(#14263),#268);
#250=STYLED_ITEM('',(#14263),#269);
#251=STYLED_ITEM('',(#14263),#270);
#252=STYLED_ITEM('',(#14263),#271);
#253=STYLED_ITEM('',(#14264),#5964);
#254=STYLED_ITEM('',(#14264),#5965);
#255=STYLED_ITEM('',(#14264),#5966);
#256=STYLED_ITEM('',(#14264),#5967);
#257=STYLED_ITEM('',(#14264),#5968);
#258=STYLED_ITEM('',(#14264),#5969);
#259=STYLED_ITEM('',(#14263),#272);
#260=STYLED_ITEM('',(#14263),#273);
#261=STYLED_ITEM('',(#14263),#274);
#262=STYLED_ITEM('',(#14263),#275);
#263=STYLED_ITEM('',(#14263),#276);
#264=STYLED_ITEM('',(#14263),#277);
#265=STYLED_ITEM('',(#14263),#278);
#266=MANIFOLD_SOLID_BREP('Base Plate',#6134);
#267=MANIFOLD_SOLID_BREP('Back Lid',#6135);
#268=MANIFOLD_SOLID_BREP('Front Tightener',#6136);
#269=MANIFOLD_SOLID_BREP('Top (1)',#6137);
#270=MANIFOLD_SOLID_BREP('Top (2)',#6138);
#271=MANIFOLD_SOLID_BREP('Top (3)',#6139);
#272=MANIFOLD_SOLID_BREP('Top (4)',#6140);
#273=MANIFOLD_SOLID_BREP('Nozzle 60',#6141);
#274=MANIFOLD_SOLID_BREP('Nozzle 45',#6142);
#275=MANIFOLD_SOLID_BREP('Nozzle 75',#6143);
#276=MANIFOLD_SOLID_BREP('Nozzle 90',#6144);
#277=MANIFOLD_SOLID_BREP('Sprinkler',#6145);
#278=MANIFOLD_SOLID_BREP('Connector',#6146);
#279=B_SPLINE_SURFACE_WITH_KNOTS('',3,1,((#9488,#9489),(#9490,#9491),(#9492,
#9493),(#9494,#9495),(#9496,#9497),(#9498,#9499),(#9500,#9501),(#9502,#9503),
(#9504,#9505),(#9506,#9507),(#9508,#9509),(#9510,#9511),(#9512,#9513),(#9514,
#9515),(#9516,#9517),(#9518,#9519),(#9520,#9521),(#9522,#9523),(#9524,#9525),
(#9526,#9527),(#9528,#9529),(#9530,#9531),(#9532,#9533),(#9534,#9535),(#9536,
#9537),(#9538,#9539),(#9540,#9541),(#9542,#9543),(#9544,#9545),(#9546,#9547)),
 .UNSPECIFIED.,.F.,.F.,.F.,(4,2,2,2,2,2,2,2,2,2,2,2,2,2,4),(2,2),(0.,0.125000000000001,
0.1875,0.25,0.3125,0.375,0.4375,0.5,0.5625,0.625,0.6875,0.75,0.8125,0.875,
1.),(0.,1.00875859451262),.UNSPECIFIED.);
#280=B_SPLINE_SURFACE_WITH_KNOTS('',3,1,((#9560,#9561),(#9562,#9563),(#9564,
#9565),(#9566,#9567),(#9568,#9569),(#9570,#9571),(#9572,#9573),(#9574,#9575),
(#9576,#9577),(#9578,#9579),(#9580,#9581),(#9582,#9583),(#9584,#9585),(#9586,
#9587),(#9588,#9589),(#9590,#9591),(#9592,#9593),(#9594,#9595),(#9596,#9597),
(#9598,#9599),(#9600,#9601),(#9602,#9603),(#9604,#9605),(#9606,#9607),(#9608,
#9609),(#9610,#9611),(#9612,#9613),(#9614,#9615),(#9616,#9617),(#9618,#9619)),
 .UNSPECIFIED.,.F.,.F.,.F.,(4,2,2,2,2,2,2,2,2,2,2,2,2,2,4),(2,2),(0.,0.125,
0.1875,0.25,0.312499999999999,0.374999999999999,0.437499999999999,0.499999999999999,
0.562499999999999,0.624999999999999,0.687499999999999,0.75,0.8125,0.875,
1.),(0.,1.00875859529089),.UNSPECIFIED.);
#281=B_SPLINE_SURFACE_WITH_KNOTS('',3,1,((#9630,#9631),(#9632,#9633),(#9634,
#9635),(#9636,#9637),(#9638,#9639),(#9640,#9641),(#9642,#9643),(#9644,#9645),
(#9646,#9647),(#9648,#9649),(#9650,#9651),(#9652,#9653),(#9654,#9655),(#9656,
#9657),(#9658,#9659),(#9660,#9661),(#9662,#9663),(#9664,#9665),(#9666,#9667),
(#9668,#9669),(#9670,#9671),(#9672,#9673),(#9674,#9675),(#9676,#9677),(#9678,
#9679),(#9680,#9681),(#9682,#9683),(#9684,#9685),(#9686,#9687),(#9688,#9689),
(#9690,#9691),(#9692,#9693),(#9694,#9695),(#9696,#9697)),.UNSPECIFIED.,
 .F.,.F.,.F.,(4,2,2,2,2,2,2,2,2,2,2,2,2,2,2,2,4),(2,2),(0.,0.0625,0.125,
0.1875,0.25,0.3125,0.375,0.4375,0.5,0.5625,0.625,0.6875,0.75,0.8125,0.875,
0.9375,1.),(0.,1.),.UNSPECIFIED.);
#282=B_SPLINE_SURFACE_WITH_KNOTS('',3,1,((#9723,#9724),(#9725,#9726),(#9727,
#9728),(#9729,#9730)),.UNSPECIFIED.,.F.,.F.,.F.,(4,4),(2,2),(0.14457615148808,
1.),(0.,1.2),.UNSPECIFIED.);
#283=B_SPLINE_SURFACE_WITH_KNOTS('',3,1,((#9770,#9771),(#9772,#9773),(#9774,
#9775),(#9776,#9777)),.UNSPECIFIED.,.F.,.F.,.F.,(4,4),(2,2),(0.,0.855423965834485),
(0.,1.2),.UNSPECIFIED.);
#284=B_SPLINE_SURFACE_WITH_KNOTS('',3,1,((#9934,#9935),(#9936,#9937),(#9938,
#9939),(#9940,#9941),(#9942,#9943),(#9944,#9945),(#9946,#9947),(#9948,#9949),
(#9950,#9951),(#9952,#9953),(#9954,#9955),(#9956,#9957),(#9958,#9959),(#9960,
#9961),(#9962,#9963),(#9964,#9965),(#9966,#9967),(#9968,#9969),(#9970,#9971),
(#9972,#9973),(#9974,#9975),(#9976,#9977),(#9978,#9979),(#9980,#9981),(#9982,
#9983),(#9984,#9985),(#9986,#9987),(#9988,#9989),(#9990,#9991),(#9992,#9993)),
 .UNSPECIFIED.,.F.,.F.,.F.,(4,2,2,2,2,2,2,2,2,2,2,2,2,2,4),(2,2),(0.,0.125000000000001,
0.1875,0.25,0.3125,0.375,0.4375,0.5,0.5625,0.625,0.6875,0.75,0.8125,0.875,
1.),(0.,1.00875859388372),.UNSPECIFIED.);
#285=B_SPLINE_SURFACE_WITH_KNOTS('',3,1,((#9999,#10000),(#10001,#10002),
(#10003,#10004),(#10005,#10006),(#10007,#10008),(#10009,#10010),(#10011,
#10012),(#10013,#10014),(#10015,#10016),(#10017,#10018),(#10019,#10020),
(#10021,#10022),(#10023,#10024),(#10025,#10026),(#10027,#10028),(#10029,
#10030),(#10031,#10032),(#10033,#10034),(#10035,#10036),(#10037,#10038),
(#10039,#10040),(#10041,#10042),(#10043,#10044),(#10045,#10046),(#10047,
#10048),(#10049,#10050),(#10051,#10052),(#10053,#10054),(#10055,#10056),
(#10057,#10058)),.UNSPECIFIED.,.F.,.F.,.F.,(4,2,2,2,2,2,2,2,2,2,2,2,2,2,
4),(2,2),(0.,0.125,0.1875,0.25,0.312499999999999,0.374999999999999,0.437499999999999,
0.499999999999999,0.562499999999999,0.624999999999999,0.687499999999999,
0.75,0.8125,0.875,1.),(0.,1.00875859641008),.UNSPECIFIED.);
#286=B_SPLINE_SURFACE_WITH_KNOTS('',3,1,((#10064,#10065),(#10066,#10067),
(#10068,#10069),(#10070,#10071),(#10072,#10073),(#10074,#10075),(#10076,
#10077),(#10078,#10079),(#10080,#10081),(#10082,#10083),(#10084,#10085),
(#10086,#10087),(#10088,#10089),(#10090,#10091),(#10092,#10093),(#10094,
#10095),(#10096,#10097),(#10098,#10099),(#10100,#10101),(#10102,#10103),
(#10104,#10105),(#10106,#10107),(#10108,#10109),(#10110,#10111),(#10112,
#10113),(#10114,#10115),(#10116,#10117),(#10118,#10119),(#10120,#10121),
(#10122,#10123),(#10124,#10125),(#10126,#10127),(#10128,#10129),(#10130,
#10131)),.UNSPECIFIED.,.F.,.F.,.F.,(4,2,2,2,2,2,2,2,2,2,2,2,2,2,2,2,4),
(2,2),(0.,0.0625,0.125,0.1875,0.25,0.3125,0.375,0.4375,0.5,0.5625,0.625,
0.6875,0.75,0.8125,0.875,0.9375,1.),(0.,1.),.UNSPECIFIED.);
#287=B_SPLINE_SURFACE_WITH_KNOTS('',3,1,((#10132,#10133),(#10134,#10135),
(#10136,#10137),(#10138,#10139)),.UNSPECIFIED.,.F.,.F.,.F.,(4,4),(2,2),
(0.144576151499063,1.),(0.,1.20000000000001),.UNSPECIFIED.);
#288=B_SPLINE_SURFACE_WITH_KNOTS('',3,1,((#10140,#10141),(#10142,#10143),
(#10144,#10145),(#10146,#10147)),.UNSPECIFIED.,.F.,.F.,.F.,(4,4),(2,2),
(0.,0.855423965822116),(0.,1.2),.UNSPECIFIED.);
#289=B_SPLINE_SURFACE_WITH_KNOTS('',3,1,((#13841,#13842),(#13843,#13844),
(#13845,#13846),(#13847,#13848),(#13849,#13850),(#13851,#13852),(#13853,
#13854),(#13855,#13856),(#13857,#13858),(#13859,#13860),(#13861,#13862)),
 .UNSPECIFIED.,.F.,.F.,.F.,(4,1,1,1,1,1,1,1,4),(2,2),(3.14159265358979,
3.53429173528852,3.92699081698724,4.31968989868597,4.71238898038469,5.10508806208341,
5.49778714378214,5.89048622548086,6.28318530717959),(0.,0.129347179873149),
 .UNSPECIFIED.);
#290=B_SPLINE_SURFACE_WITH_KNOTS('',3,1,((#13904,#13905),(#13906,#13907),
(#13908,#13909),(#13910,#13911),(#13912,#13913),(#13914,#13915),(#13916,
#13917),(#13918,#13919),(#13920,#13921),(#13922,#13923),(#13924,#13925)),
 .UNSPECIFIED.,.F.,.F.,.F.,(4,1,1,1,1,1,1,1,4),(2,2),(3.14159265358979,
3.53429173528851,3.92699081698724,4.31968989868596,4.71238898038469,5.10508806208341,
5.49778714378214,5.89048622548086,6.28318530717959),(0.,0.129347179873148),
 .UNSPECIFIED.);
#291=B_SPLINE_SURFACE_WITH_KNOTS('',3,1,((#13967,#13968),(#13969,#13970),
(#13971,#13972),(#13973,#13974),(#13975,#13976),(#13977,#13978),(#13979,
#13980),(#13981,#13982),(#13983,#13984),(#13985,#13986),(#13987,#13988)),
 .UNSPECIFIED.,.F.,.F.,.F.,(4,1,1,1,1,1,1,1,4),(2,2),(3.14159265358979,
3.53429173528851,3.92699081698723,4.31968989868596,4.71238898038468,5.10508806208341,
5.49778714378213,5.89048622548085,6.28318530717958),(0.,0.129347179873145),
 .UNSPECIFIED.);
#292=B_SPLINE_CURVE_WITH_KNOTS('',3,(#8671,#8672,#8673,#8674,#8675,#8676,
#8677,#8678,#8679,#8680,#8681,#8682,#8683,#8684,#8685,#8686,#8687,#8688,
#8689,#8690,#8691,#8692,#8693,#8694,#8695,#8696,#8697,#8698,#8699,#8700,
#8701,#8702,#8703,#8704,#8705,#8706,#8707,#8708),.UNSPECIFIED.,.F.,.F.,
(4,2,2,2,2,2,2,2,2,2,2,2,2,2,2,2,2,2,4),(0.,0.0927340025111304,0.185468005022261,
0.370936010044522,0.741872020089043,1.11280803013356,1.48374404017809,2.05783904851561,
2.34488655268438,2.63193405685314,2.9189815610219,3.20602906519066,3.78012407352819,
4.15106008357271,4.52199609361724,4.89293210366176,5.07840010868402,5.17113411119515,
5.26386811370629),.UNSPECIFIED.);
#293=B_SPLINE_CURVE_WITH_KNOTS('',3,(#8709,#8710,#8711,#8712,#8713,#8714,
#8715,#8716,#8717,#8718,#8719,#8720,#8721,#8722,#8723,#8724,#8725,#8726,
#8727,#8728,#8729,#8730,#8731,#8732,#8733,#8734,#8735,#8736,#8737,#8738,
#8739,#8740,#8741,#8742,#8743,#8744,#8745,#8746),.UNSPECIFIED.,.F.,.F.,
(4,2,2,2,2,2,2,2,2,2,2,2,2,2,2,2,2,2,4),(5.26386811370629,5.35660211621742,
5.44933611872855,5.63480412375081,6.00574013379534,6.37667614383986,6.74761215388439,
7.32170716222191,7.60875466639068,7.89580217055944,8.1828496747282,8.46989717889697,
9.0439921872345,9.41492819727902,9.78586420732354,10.1568002173681,10.3422682223903,
10.4350022249015,10.5277362274126),.UNSPECIFIED.);
#294=B_SPLINE_CURVE_WITH_KNOTS('',3,(#8749,#8750,#8751,#8752,#8753,#8754,
#8755,#8756,#8757,#8758,#8759,#8760,#8761,#8762,#8763,#8764,#8765,#8766,
#8767,#8768,#8769,#8770,#8771,#8772,#8773,#8774,#8775,#8776,#8777,#8778,
#8779,#8780,#8781,#8782,#8783,#8784,#8785,#8786),.UNSPECIFIED.,.F.,.F.,
(4,2,2,2,2,2,2,2,2,2,2,2,2,2,2,2,2,2,4),(0.,0.0927340025111308,0.185468005022262,
0.370936010044523,0.741872020089046,1.11280803013357,1.48374404017809,2.05783904851562,
2.34488655268438,2.63193405685315,2.91898156102191,3.20602906519068,3.7801240735282,
4.15106008357273,4.52199609361725,4.89293210366178,5.07840010868404,5.17113411119517,
5.2638681137063),.UNSPECIFIED.);
#295=B_SPLINE_CURVE_WITH_KNOTS('',3,(#8787,#8788,#8789,#8790,#8791,#8792,
#8793,#8794,#8795,#8796,#8797,#8798,#8799,#8800,#8801,#8802,#8803,#8804,
#8805,#8806,#8807,#8808,#8809,#8810,#8811,#8812,#8813,#8814,#8815,#8816,
#8817,#8818,#8819,#8820,#8821,#8822,#8823,#8824),.UNSPECIFIED.,.F.,.F.,
(4,2,2,2,2,2,2,2,2,2,2,2,2,2,2,2,2,2,4),(5.2638681137063,5.35660211621743,
5.44933611872857,5.63480412375083,6.00574013379535,6.37667614383987,6.7476121538844,
7.32170716222192,7.60875466639069,7.89580217055945,8.18284967472821,8.46989717889698,
9.0439921872345,9.41492819727902,9.78586420732355,10.1568002173681,10.3422682223903,
10.4350022249015,10.5277362274126),.UNSPECIFIED.);
#296=B_SPLINE_CURVE_WITH_KNOTS('',3,(#8834,#8835,#8836,#8837,#8838,#8839,
#8840,#8841,#8842,#8843,#8844,#8845,#8846,#8847,#8848,#8849,#8850,#8851),
 .UNSPECIFIED.,.F.,.F.,(4,2,2,2,2,2,2,2,4),(9.15255602234747,9.53372020064684,
9.91488437894621,10.2960485572456,10.6772127355449,11.0587615591079,11.4403103826708,
11.8218592062337,12.2034080297966),.UNSPECIFIED.);
#297=B_SPLINE_CURVE_WITH_KNOTS('',3,(#8853,#8854,#8855,#8856,#8857,#8858,
#8859,#8860,#8861,#8862,#8863,#8864,#8865,#8866,#8867,#8868,#8869,#8870),
 .UNSPECIFIED.,.F.,.F.,(4,2,2,2,2,2,2,2,4),(6.10170401489831,6.48325283846123,
6.86480166202415,7.24635048558707,7.62789930914999,8.00906348744936,8.39022766574873,
8.7713918440481,9.15255602234747),.UNSPECIFIED.);
#298=B_SPLINE_CURVE_WITH_KNOTS('',3,(#8878,#8879,#8880,#8881,#8882,#8883,
#8884,#8885,#8886,#8887,#8888,#8889,#8890,#8891,#8892,#8893,#8894,#8895,
#8896,#8897,#8898,#8899,#8900,#8901,#8902),.UNSPECIFIED.,.F.,.F.,(4,3,3,
3,3,3,3,3,4),(-1.,-0.875,-0.75,-0.625,-0.5,-0.375,-0.25,-0.125,0.),
 .UNSPECIFIED.);
#299=B_SPLINE_CURVE_WITH_KNOTS('',3,(#8935,#8936,#8937,#8938,#8939,#8940,
#8941,#8942,#8943,#8944,#8945,#8946,#8947,#8948,#8949,#8950,#8951,#8952,
#8953,#8954,#8955,#8956,#8957,#8958,#8959,#8960,#8961,#8962,#8963,#8964,
#8965,#8966,#8967,#8968,#8969,#8970,#8971,#8972,#8973,#8974,#8975,#8976,
#8977,#8978,#8979,#8980,#8981,#8982,#8983,#8984,#8985,#8986,#8987,#8988,
#8989,#8990,#8991,#8992,#8993,#8994,#8995,#8996,#8997,#8998,#8999,#9000,
#9001,#9002,#9003,#9004,#9005,#9006,#9007,#9008,#9009,#9010,#9011,#9012,
#9013,#9014,#9015,#9016,#9017,#9018,#9019,#9020,#9021,#9022,#9023,#9024,
#9025,#9026,#9027,#9028,#9029,#9030,#9031,#9032,#9033,#9034,#9035,#9036,
#9037,#9038,#9039,#9040,#9041,#9042,#9043,#9044,#9045,#9046,#9047,#9048,
#9049,#9050,#9051,#9052,#9053,#9054,#9055,#9056,#9057,#9058,#9059,#9060,
#9061,#9062,#9063,#9064,#9065,#9066,#9067,#9068,#9069,#9070,#9071,#9072,
#9073,#9074,#9075,#9076,#9077,#9078,#9079,#9080,#9081,#9082,#9083,#9084,
#9085,#9086,#9087,#9088,#9089,#9090,#9091,#9092,#9093,#9094,#9095,#9096,
#9097,#9098,#9099,#9100,#9101,#9102,#9103,#9104,#9105,#9106,#9107,#9108,
#9109,#9110,#9111,#9112,#9113,#9114,#9115,#9116,#9117,#9118),
 .UNSPECIFIED.,.F.,.F.,(4,3,3,3,3,3,3,3,3,3,3,3,3,3,3,3,3,3,3,3,3,3,3,3,
3,3,3,3,3,3,3,3,3,3,3,3,3,3,3,3,3,3,3,3,3,3,3,3,3,3,3,3,3,3,3,3,3,3,3,3,
3,4),(0.150241198747907,0.167397304835228,0.184718118887321,0.202241047709381,
0.220007464163269,0.238064286953153,0.24996953246951,0.25115288079109,0.277756413628116,
0.304952901732967,0.332851547605054,0.361595243786114,0.371570318101956,
0.374891379875467,0.37684512588001,0.404565053134646,0.433143322897528,
0.46278930680584,0.493811743368577,0.49776633912351,0.499650446210555,0.501139153619483,
0.526262386397414,0.552281259081706,0.580263680389099,0.606497200364781,
0.618794162853381,0.622041027561349,0.623773539268005,0.624868539292833,
0.62607780545653,0.662083917086729,0.720106829170489,0.737600152347333,
0.745800147586479,0.747905908951524,0.749388388026565,0.749955707873429,
0.750554094407055,0.771533017768898,0.793328350135385,0.806245328251924,
0.812300161744051,0.812901601299671,0.828591002192834,0.846067273157757,
0.865308864013037,0.873727060012223,0.874713567355877,0.87499463526931,
0.875252029008748,0.898077041623502,0.91317689673975,0.926104230971432,
0.935341202100003,0.937361789534378,0.937508712583833,0.949516479167898,
0.963001489246603,0.977729187677142,0.995717213427348,1.),.UNSPECIFIED.);
#300=B_SPLINE_CURVE_WITH_KNOTS('',3,(#9125,#9126,#9127,#9128,#9129,#9130,
#9131,#9132,#9133,#9134,#9135,#9136,#9137,#9138,#9139,#9140,#9141,#9142,
#9143,#9144,#9145,#9146,#9147,#9148,#9149,#9150,#9151,#9152,#9153,#9154,
#9155,#9156,#9157,#9158,#9159,#9160,#9161,#9162,#9163,#9164,#9165,#9166,
#9167,#9168,#9169,#9170,#9171,#9172,#9173,#9174,#9175,#9176,#9177,#9178,
#9179,#9180,#9181,#9182,#9183,#9184,#9185,#9186,#9187,#9188,#9189,#9190,
#9191,#9192,#9193,#9194,#9195,#9196,#9197,#9198,#9199,#9200,#9201,#9202,
#9203,#9204,#9205,#9206,#9207,#9208,#9209,#9210,#9211,#9212,#9213,#9214,
#9215,#9216,#9217,#9218,#9219,#9220,#9221,#9222,#9223,#9224,#9225,#9226,
#9227,#9228,#9229,#9230,#9231,#9232,#9233,#9234,#9235,#9236,#9237,#9238,
#9239,#9240,#9241,#9242,#9243,#9244,#9245,#9246,#9247,#9248,#9249,#9250,
#9251,#9252,#9253,#9254,#9255,#9256,#9257,#9258,#9259,#9260,#9261,#9262,
#9263,#9264,#9265,#9266,#9267,#9268,#9269,#9270,#9271,#9272,#9273,#9274,
#9275,#9276,#9277,#9278,#9279,#9280,#9281,#9282,#9283,#9284,#9285,#9286,
#9287,#9288,#9289,#9290,#9291,#9292,#9293,#9294,#9295,#9296,#9297,#9298,
#9299,#9300,#9301,#9302,#9303,#9304,#9305),.UNSPECIFIED.,.F.,.F.,(4,3,3,
3,3,3,3,3,3,3,3,3,3,3,3,3,3,3,3,3,3,3,3,3,3,3,3,3,3,3,3,3,3,3,3,3,3,3,3,
3,3,3,3,3,3,3,3,3,3,3,3,3,3,3,3,3,3,3,3,3,4),(0.,0.0173864418603424,0.0317406407068232,
0.0445735019151384,0.0571545623287322,0.0602506826648901,0.0617926957229375,
0.0622286000993027,0.0624303599347524,0.062594733958677,0.0746665408516836,
0.0885152798747999,0.106661753514485,0.118272684996839,0.12398744033581,
0.12469708287651,0.124978108020046,0.125243557342601,0.14788473893768,0.165674472900084,
0.181276305626835,0.186498845179634,0.187421439977098,0.188081999482287,
0.210113337373066,0.230102338342194,0.249466683031036,0.250074016598888,
0.290650259758732,0.333611006225432,0.365870403860414,0.373431200181113,
0.37495605866907,0.376045195512328,0.405652456316879,0.433409263321146,
0.459431269887646,0.483826901043739,0.495262353148158,0.498872802540326,
0.501065640438556,0.531952057906504,0.561479569871501,0.589959832895018,
0.617600948986098,0.624836289376345,0.626872446293665,0.655342990004338,
0.683068491132681,0.710166098531947,0.73672700441613,0.743791652164193,
0.747103205796098,0.748975108318689,0.750181999132194,0.768352317329036,
0.786243445752231,0.803790273865076,0.82117579398772,0.838357975229974,
0.849761368385144),.UNSPECIFIED.);
#301=B_SPLINE_CURVE_WITH_KNOTS('',3,(#9309,#9310,#9311,#9312),
 .UNSPECIFIED.,.F.,.F.,(4,4),(0.149678083001057,0.999999081493329),
 .UNSPECIFIED.);
#302=B_SPLINE_CURVE_WITH_KNOTS('',3,(#9316,#9317,#9318,#9319),
 .UNSPECIFIED.,.F.,.F.,(4,4),(1.03512807303671E-6,0.850322033620394),
 .UNSPECIFIED.);
#303=B_SPLINE_CURVE_WITH_KNOTS('',3,(#9322,#9323,#9324,#9325),
 .UNSPECIFIED.,.F.,.F.,(4,4),(-1.,-0.850320998496977),.UNSPECIFIED.);
#304=B_SPLINE_CURVE_WITH_KNOTS('',3,(#9330,#9331,#9332,#9333,#9334,#9335),
 .UNSPECIFIED.,.F.,.F.,(4,2,4),(0.,0.125000000000001,0.149679001503013),
 .UNSPECIFIED.);
#305=B_SPLINE_CURVE_WITH_KNOTS('',3,(#9339,#9340,#9341,#9342,#9343,#9344,
#9345,#9346,#9347,#9348,#9349,#9350,#9351,#9352,#9353,#9354,#9355,#9356,
#9357,#9358,#9359,#9360,#9361,#9362,#9363,#9364,#9365,#9366,#9367,#9368,
#9369,#9370,#9371,#9372,#9373,#9374,#9375,#9376,#9377,#9378,#9379,#9380,
#9381,#9382,#9383,#9384),.UNSPECIFIED.,.F.,.F.,(4,3,3,3,3,3,3,3,3,3,3,3,
3,3,3,4),(-16.2042554582664,-16.1371180260605,-14.2967993206844,-13.2982156828388,
-12.2761212402173,-11.2362598068131,-10.1850784450982,-9.12964303443693,
-8.07313766648818,-7.01663510715248,-5.96496475382742,-4.92301254140941,
-3.89517570042547,-2.88556286360814,-1.89741455218585,0.),.UNSPECIFIED.);
#306=B_SPLINE_CURVE_WITH_KNOTS('',3,(#9390,#9391,#9392,#9393,#9394,#9395,
#9396,#9397,#9398,#9399,#9400,#9401,#9402,#9403,#9404,#9405,#9406,#9407,
#9408,#9409,#9410,#9411,#9412,#9413,#9414,#9415,#9416,#9417,#9418,#9419,
#9420,#9421,#9422,#9423,#9424,#9425,#9426,#9427,#9428,#9429,#9430,#9431,
#9432,#9433,#9434,#9435),.UNSPECIFIED.,.F.,.F.,(4,3,3,3,3,3,3,3,3,3,3,3,
3,3,3,4),(-0.0671460795128853,0.,1.84055573902674,2.83926799475898,3.86149408346386,
4.90148945134311,5.95280620554087,7.00837755660534,8.06501900276707,9.12165763995372,
10.1734634487402,11.2155498649205,12.2435190916037,13.2532619668624,14.2415375520883,
16.1391964918471),.UNSPECIFIED.);
#307=B_SPLINE_CURVE_WITH_KNOTS('',3,(#9439,#9440,#9441,#9442,#9443,#9444,
#9445,#9446,#9447,#9448,#9449,#9450,#9451,#9452,#9453,#9454,#9455,#9456,
#9457,#9458,#9459,#9460,#9461,#9462,#9463,#9464,#9465,#9466,#9467,#9468,
#9469,#9470,#9471,#9472,#9473,#9474,#9475,#9476,#9477,#9478,#9479,#9480,
#9481,#9482,#9483,#9484,#9485,#9486,#9487),.UNSPECIFIED.,.F.,.F.,(4,3,3,
3,3,3,3,3,3,3,3,3,3,3,3,3,4),(0.,0.0625,0.125,0.1875,0.25,0.3125,0.375,
0.4375,0.5,0.5625,0.625,0.6875,0.75,0.8125,0.875,0.9375,1.),
 .UNSPECIFIED.);
#308=B_SPLINE_CURVE_WITH_KNOTS('',3,(#9549,#9550,#9551,#9552),
 .UNSPECIFIED.,.F.,.F.,(4,4),(-1.,-0.149679001507915),.UNSPECIFIED.);
#309=B_SPLINE_CURVE_WITH_KNOTS('',3,(#9554,#9555,#9556,#9557,#9558,#9559),
 .UNSPECIFIED.,.F.,.F.,(4,2,4),(0.,0.125000000000001,0.149679001507905),
 .UNSPECIFIED.);
#310=B_SPLINE_CURVE_WITH_KNOTS('',3,(#9620,#9621,#9622,#9623),
 .UNSPECIFIED.,.F.,.F.,(4,4),(-1.,-0.850320998492047),.UNSPECIFIED.);
#311=B_SPLINE_CURVE_WITH_KNOTS('',3,(#9626,#9627,#9628,#9629),
 .UNSPECIFIED.,.F.,.F.,(4,4),(-0.850320998492047,0.),.UNSPECIFIED.);
#312=B_SPLINE_CURVE_WITH_KNOTS('',3,(#9698,#9699,#9700,#9701,#9702,#9703,
#9704,#9705,#9706,#9707,#9708,#9709,#9710,#9711,#9712,#9713,#9714,#9715,
#9716,#9717,#9718,#9719,#9720,#9721,#9722),.UNSPECIFIED.,.F.,.F.,(4,3,3,
3,3,3,3,3,4),(-1.,-0.875,-0.75,-0.625,-0.5,-0.375,-0.25,-0.125,0.),
 .UNSPECIFIED.);
#313=B_SPLINE_CURVE_WITH_KNOTS('',3,(#9734,#9735,#9736,#9737,#9738,#9739,
#9740,#9741,#9742,#9743,#9744,#9745,#9746,#9747,#9748,#9749,#9750,#9751,
#9752,#9753,#9754,#9755,#9756,#9757,#9758,#9759,#9760,#9761,#9762,#9763,
#9764,#9765,#9766,#9767),.UNSPECIFIED.,.F.,.F.,(4,2,2,2,2,2,2,2,2,2,2,2,
2,2,2,2,4),(0.,0.38154882356292,0.76309764712584,1.14464647068876,1.52619529425168,
1.90735947255105,2.28852365085042,2.66968782914979,3.05085200744916,3.43201618574853,
3.8131803640479,4.19434454234727,4.57550872064664,4.95705754420956,5.33860636777248,
5.72015519133539,6.10170401489832),.UNSPECIFIED.);
#314=B_SPLINE_CURVE_WITH_KNOTS('',3,(#9788,#9789,#9790,#9791,#9792,#9793,
#9794,#9795,#9796,#9797,#9798,#9799,#9800,#9801,#9802,#9803,#9804,#9805,
#9806,#9807,#9808,#9809,#9810,#9811,#9812,#9813,#9814,#9815,#9816,#9817,
#9818,#9819,#9820,#9821,#9822,#9823,#9824,#9825,#9826,#9827,#9828,#9829,
#9830,#9831,#9832,#9833),.UNSPECIFIED.,.F.,.F.,(4,3,3,3,3,3,3,3,3,3,3,3,
3,3,3,4),(-16.2042554581874,-16.1371180259159,-14.2967993206444,-13.2982156828138,
-12.2761212402042,-11.2362598068085,-10.1850784450988,-9.12964303443895,
-8.07313766648923,-7.01663510715275,-5.96496475382618,-4.92301254140818,
-3.89517570042437,-2.88556286360765,-1.89741455218581,0.),.UNSPECIFIED.);
#315=B_SPLINE_CURVE_WITH_KNOTS('',3,(#9837,#9838,#9839,#9840,#9841,#9842,
#9843,#9844,#9845,#9846,#9847,#9848,#9849,#9850,#9851,#9852,#9853,#9854,
#9855,#9856,#9857,#9858,#9859,#9860,#9861,#9862,#9863,#9864,#9865,#9866,
#9867,#9868,#9869,#9870,#9871,#9872,#9873,#9874,#9875,#9876,#9877,#9878,
#9879,#9880,#9881,#9882),.UNSPECIFIED.,.F.,.F.,(4,3,3,3,3,3,3,3,3,3,3,3,
3,3,3,4),(-0.0671460794643839,0.,1.84055573907213,2.83926799479983,3.86149408349817,
4.9014894513689,5.95280620555617,7.00837755660805,8.06501900275524,9.12165763992751,
10.1734634486996,11.215549864865,12.2435190915338,13.2532619667787,14.2415375519915,
16.1391964917245),.UNSPECIFIED.);
#316=B_SPLINE_CURVE_WITH_KNOTS('',3,(#9885,#9886,#9887,#9888,#9889,#9890,
#9891,#9892,#9893,#9894,#9895,#9896,#9897,#9898,#9899,#9900,#9901,#9902,
#9903,#9904,#9905,#9906,#9907,#9908,#9909,#9910,#9911,#9912,#9913,#9914,
#9915,#9916,#9917,#9918,#9919,#9920,#9921,#9922,#9923,#9924,#9925,#9926,
#9927,#9928,#9929,#9930,#9931,#9932,#9933),.UNSPECIFIED.,.F.,.F.,(4,3,3,
3,3,3,3,3,3,3,3,3,3,3,3,3,4),(0.,0.0625,0.125,0.1875,0.25,0.3125,0.375,
0.4375,0.5,0.5625,0.625,0.6875,0.75,0.8125,0.875,0.9375,1.),
 .UNSPECIFIED.);
#317=B_SPLINE_CURVE_WITH_KNOTS('',3,(#9994,#9995,#9996,#9997),
 .UNSPECIFIED.,.F.,.F.,(4,4),(-1.,-0.149679001503023),.UNSPECIFIED.);
#318=B_SPLINE_CURVE_WITH_KNOTS('',3,(#10059,#10060,#10061,#10062),
 .UNSPECIFIED.,.F.,.F.,(4,4),(-0.850320998496977,0.),.UNSPECIFIED.);
#319=B_SPLINE_CURVE_WITH_KNOTS('',3,(#10199,#10200,#10201,#10202,#10203,
#10204,#10205,#10206),.UNSPECIFIED.,.F.,.F.,(4,2,2,4),(-1.01270550863141,
-0.972225883052009,-0.93592471729076,-0.9302261633243),.UNSPECIFIED.);
#320=B_SPLINE_CURVE_WITH_KNOTS('',3,(#10208,#10209,#10210,#10211,#10212,
#10213,#10214,#10215,#10216,#10217,#10218,#10219,#10220,#10221,#10222,#10223,
#10224,#10225,#10226,#10227,#10228,#10229),.UNSPECIFIED.,.F.,.F.,(4,2,2,
2,2,2,2,2,2,2,4),(0.770301299294677,0.776837516381544,0.810179859704117,
0.863854547164407,0.965601485426607,1.16658222290299,1.71041595764289,2.04547866914785,
2.21675572625692,2.31744906128486,2.32707423972487),.UNSPECIFIED.);
#321=B_SPLINE_CURVE_WITH_KNOTS('',3,(#10235,#10236,#10237,#10238,#10239,
#10240,#10241,#10242,#10243,#10244,#10245,#10246,#10247,#10248,#10249,#10250,
#10251,#10252,#10253,#10254,#10255,#10256,#10257,#10258,#10259),
 .UNSPECIFIED.,.F.,.F.,(4,2,2,2,2,3,2,2,2,2,2,4),(-0.9302261633243,-0.897559179923855,
-0.841033612998941,-0.72014052841894,-0.534875041413907,0.,0.287237711284631,
0.543909079429507,0.657892073847931,0.715678915934471,0.748705009105826,
0.770301299294677),.UNSPECIFIED.);
#322=B_SPLINE_CURVE_WITH_KNOTS('',3,(#10293,#10294,#10295,#10296,#10297,
#10298,#10299,#10300,#10301,#10302,#10303,#10304,#10305,#10306,#10307,#10308,
#10309,#10310,#10311,#10312,#10313,#10314,#10315,#10316,#10317,#10318,#10319,
#10320,#10321,#10322,#10323,#10324,#10325,#10326,#10327,#10328,#10329,#10330,
#10331,#10332,#10333,#10334,#10335,#10336),.UNSPECIFIED.,.T.,.F.,(4,2,2,
2,2,2,2,2,2,2,2,2,2,2,2,2,2,2,2,2,2,4),(-3.33977974833692,-3.05254203705232,
-2.79587066890727,-2.68188767448872,-2.62410083240212,-2.59107473923068,
-2.56294223195498,-2.52959988863245,-2.47592520117237,-2.37417826291126,
-2.17319752543706,-1.62936379070288,-1.29430107920164,-1.12302402209434,
-1.02233068706724,-0.972225883048282,-0.935924717287512,-0.897559179921191,
-0.841033612997187,-0.720140528418584,-0.534875041413949,0.),
 .UNSPECIFIED.);
#323=B_SPLINE_CURVE_WITH_KNOTS('',3,(#10338,#10339,#10340,#10341,#10342,
#10343,#10344,#10345,#10346,#10347,#10348,#10349,#10350,#10351,#10352,#10353,
#10354,#10355,#10356,#10357,#10358,#10359,#10360,#10361,#10362,#10363,#10364,
#10365,#10366,#10367,#10368,#10369,#10370,#10371,#10372,#10373,#10374,#10375,
#10376,#10377,#10378,#10379,#10380,#10381),.UNSPECIFIED.,.T.,.F.,(4,2,2,
2,2,2,2,2,2,2,2,2,2,2,2,2,2,2,2,2,2,4),(-3.3397797483622,-3.05254203707762,
-2.79587066893242,-2.68188767451365,-2.62410083242683,-2.5910747392553,
-2.5629422319795,-2.52959988865681,-2.47592520119621,-2.37417826293345,
-2.17319752545607,-1.62936379071395,-1.29430107920719,-1.1230240220981,
-1.02233068707054,-0.972225883051298,-0.93592471729009,-0.89755917992317,
-0.841033612998203,-0.720140528418294,-0.534875041413579,0.),
 .UNSPECIFIED.);
#324=B_SPLINE_CURVE_WITH_KNOTS('',3,(#10383,#10384,#10385,#10386,#10387,
#10388,#10389,#10390,#10391,#10392,#10393,#10394,#10395,#10396,#10397,#10398,
#10399,#10400,#10401,#10402,#10403,#10404,#10405,#10406,#10407,#10408,#10409,
#10410,#10411,#10412,#10413,#10414,#10415,#10416,#10417,#10418,#10419,#10420,
#10421,#10422,#10423,#10424,#10425,#10426),.UNSPECIFIED.,.T.,.F.,(4,2,2,
2,2,2,2,2,2,2,2,2,2,2,2,2,2,2,2,2,2,4),(-3.3397797483903,-3.05254203710569,
-2.79587066896086,-2.68188767454252,-2.62410083245608,-2.59107473928483,
-2.56294223200934,-2.52959988868709,-2.47592520122646,-2.37417826296174,
-2.17319752548078,-1.62936379072977,-1.29430107921846,-1.12302402210607,
-1.02233068707609,-0.972225883055856,-0.935924717293985,-0.897559179926439,
-0.841033613000712,-0.720140528419696,-0.534875041414283,0.),
 .UNSPECIFIED.);
#325=B_SPLINE_CURVE_WITH_KNOTS('',3,(#10500,#10501,#10502,#10503,#10504,
#10505),.UNSPECIFIED.,.F.,.F.,(4,2,4),(0.661047189651573,0.682893822496354,
0.69260663288377),.UNSPECIFIED.);
#326=B_SPLINE_CURVE_WITH_KNOTS('',3,(#10509,#10510,#10511,#10512,#10513,
#10514),.UNSPECIFIED.,.F.,.F.,(4,2,4),(0.954385955540414,0.955688960187291,
0.983990255335198),.UNSPECIFIED.);
#327=B_SPLINE_CURVE_WITH_KNOTS('',3,(#10518,#10519,#10520,#10521,#10522,
#10523),.UNSPECIFIED.,.F.,.F.,(4,2,4),(0.11431583352954,0.135832218753253,
0.145774815807224),.UNSPECIFIED.);
#328=B_SPLINE_CURVE_WITH_KNOTS('',3,(#10526,#10527,#10528,#10529,#10530,
#10531),.UNSPECIFIED.,.F.,.F.,(4,2,4),(0.406957049146252,0.408029153839697,
0.43652027355868),.UNSPECIFIED.);
#329=B_SPLINE_CURVE_WITH_KNOTS('',3,(#10537,#10538,#10539,#10540,#10541,
#10542,#10543,#10544,#10545,#10546),.UNSPECIFIED.,.F.,.F.,(4,2,2,2,4),(-0.178698063821344,
-0.13526955955559,-0.076624980274606,0.,0.000624348927189005),
 .UNSPECIFIED.);
#330=B_SPLINE_CURVE_WITH_KNOTS('',3,(#10547,#10548,#10549,#10550,#10551,
#10552,#10553,#10554,#10555,#10556),.UNSPECIFIED.,.F.,.F.,(4,2,2,2,4),(0.221433756193381,
0.257003031040665,0.305034737267452,0.367792942517405,0.3683043034075),
 .UNSPECIFIED.);
#331=B_SPLINE_CURVE_WITH_KNOTS('',3,(#10558,#10559,#10560,#10561,#10562,
#10563,#10564,#10565,#10566,#10567),.UNSPECIFIED.,.F.,.F.,(4,2,2,2,4),(-0.178698063657826,
-0.135269559443281,-0.0766249802302674,0.,0.000624348926984052),
 .UNSPECIFIED.);
#332=B_SPLINE_CURVE_WITH_KNOTS('',3,(#10569,#10570,#10571,#10572,#10573,
#10574,#10575,#10576,#10577,#10578),.UNSPECIFIED.,.F.,.F.,(4,2,2,2,4),(0.22143375619356,
0.257003031040236,0.305034737266783,0.367792942534155,0.36830430342492),
 .UNSPECIFIED.);
#333=B_SPLINE_CURVE_WITH_KNOTS('',3,(#10585,#10586,#10587,#10588,#10589,
#10590),.UNSPECIFIED.,.F.,.F.,(4,2,4),(0.661047189631137,0.682893822475484,
0.692606632862655),.UNSPECIFIED.);
#334=B_SPLINE_CURVE_WITH_KNOTS('',3,(#10594,#10595,#10596,#10597,#10598,
#10599),.UNSPECIFIED.,.F.,.F.,(4,2,4),(0.954385955875588,0.955688960523108,
0.983990255684603),.UNSPECIFIED.);
#335=B_SPLINE_CURVE_WITH_KNOTS('',3,(#10603,#10604,#10605,#10606,#10607,
#10608),.UNSPECIFIED.,.F.,.F.,(4,2,4),(0.11431583355748,0.135832218786672,
0.145774815843186),.UNSPECIFIED.);
#336=B_SPLINE_CURVE_WITH_KNOTS('',3,(#10611,#10612,#10613,#10614,#10615,
#10616),.UNSPECIFIED.,.F.,.F.,(4,2,4),(0.406957049130622,0.408029153824045,
0.436520273542523),.UNSPECIFIED.);
#337=B_SPLINE_CURVE_WITH_KNOTS('',3,(#10626,#10627,#10628,#10629,#10630,
#10631),.UNSPECIFIED.,.F.,.F.,(4,2,4),(0.661047189621191,0.682893822464398,
0.692606632851314),.UNSPECIFIED.);
#338=B_SPLINE_CURVE_WITH_KNOTS('',3,(#10635,#10636,#10637,#10638,#10639,
#10640),.UNSPECIFIED.,.F.,.F.,(4,2,4),(0.954385955650832,0.95568896029806,
0.983990255452134),.UNSPECIFIED.);
#339=B_SPLINE_CURVE_WITH_KNOTS('',3,(#10644,#10645,#10646,#10647,#10648,
#10649),.UNSPECIFIED.,.F.,.F.,(4,2,4),(0.114315833531678,0.135832218756235,
0.145774815810657),.UNSPECIFIED.);
#340=B_SPLINE_CURVE_WITH_KNOTS('',3,(#10652,#10653,#10654,#10655,#10656,
#10657),.UNSPECIFIED.,.F.,.F.,(4,2,4),(0.406957049123385,0.408029153816832,
0.43652027353595),.UNSPECIFIED.);
#341=B_SPLINE_CURVE_WITH_KNOTS('',3,(#10667,#10668,#10669,#10670,#10671,
#10672),.UNSPECIFIED.,.F.,.F.,(4,2,4),(0.661047189700789,0.682893822549002,
0.692606632937976),.UNSPECIFIED.);
#342=B_SPLINE_CURVE_WITH_KNOTS('',3,(#10676,#10677,#10678,#10679,#10680,
#10681),.UNSPECIFIED.,.F.,.F.,(4,2,4),(0.954385955972242,0.955688960619816,
0.983990255786846),.UNSPECIFIED.);
#343=B_SPLINE_CURVE_WITH_KNOTS('',3,(#10685,#10686,#10687,#10688,#10689,
#10690),.UNSPECIFIED.,.F.,.F.,(4,2,4),(0.114315833560946,0.135832218791008,
0.145774815847966),.UNSPECIFIED.);
#344=B_SPLINE_CURVE_WITH_KNOTS('',3,(#10693,#10694,#10695,#10696,#10697,
#10698),.UNSPECIFIED.,.F.,.F.,(4,2,4),(0.406957049170082,0.408029153863569,
0.436520273584039),.UNSPECIFIED.);
#345=B_SPLINE_CURVE_WITH_KNOTS('',3,(#10704,#10705,#10706,#10707,#10708,
#10709,#10710,#10711,#10712,#10713),.UNSPECIFIED.,.F.,.F.,(4,2,2,2,4),(-0.17869806353704,
-0.135269559359834,-0.0766249801970823,0.,0.000624348926732177),
 .UNSPECIFIED.);
#346=B_SPLINE_CURVE_WITH_KNOTS('',3,(#10714,#10715,#10716,#10717,#10718,
#10719,#10720,#10721,#10722,#10723),.UNSPECIFIED.,.F.,.F.,(4,2,2,2,4),(0.221433756192697,
0.257003031038445,0.305034737264325,0.3677929425703,0.368304303461073),
 .UNSPECIFIED.);
#347=B_SPLINE_CURVE_WITH_KNOTS('',3,(#10725,#10726,#10727,#10728,#10729,
#10730,#10731,#10732,#10733,#10734),.UNSPECIFIED.,.F.,.F.,(4,2,2,2,4),(-0.178698063770044,
-0.135269559520182,-0.0766249802604931,0.,0.000624348926843672),
 .UNSPECIFIED.);
#348=B_SPLINE_CURVE_WITH_KNOTS('',3,(#10736,#10737,#10738,#10739,#10740,
#10741,#10742,#10743,#10744,#10745),.UNSPECIFIED.,.F.,.F.,(4,2,2,2,4),(0.221433756193478,
0.257003031040149,0.305034737266569,0.367792942538401,0.368304303428461),
 .UNSPECIFIED.);
#349=B_SPLINE_CURVE_WITH_KNOTS('',3,(#10748,#10749,#10750,#10751,#10752,
#10753,#10754,#10755,#10756,#10757),.UNSPECIFIED.,.F.,.F.,(4,2,2,2,4),(-0.178698063553284,
-0.135269559371072,-0.0766249802015666,0.,0.000624348926677296),
 .UNSPECIFIED.);
#350=B_SPLINE_CURVE_WITH_KNOTS('',3,(#10758,#10759,#10760,#10761,#10762,
#10763,#10764,#10765,#10766,#10767),.UNSPECIFIED.,.F.,.F.,(4,2,2,2,4),(0.221433756192838,
0.25700303103897,0.305034737265084,0.367792942555533,0.368304303445851),
 .UNSPECIFIED.);
#351=B_SPLINE_CURVE_WITH_KNOTS('',3,(#10769,#10770,#10771,#10772,#10773,
#10774,#10775,#10776,#10777,#10778),.UNSPECIFIED.,.F.,.F.,(4,2,2,2,4),(-0.178698063553173,
-0.135269559370956,-0.0766249802014978,0.,0.000624348926817562),
 .UNSPECIFIED.);
#352=B_SPLINE_CURVE_WITH_KNOTS('',3,(#10780,#10781,#10782,#10783,#10784,
#10785,#10786,#10787,#10788,#10789),.UNSPECIFIED.,.F.,.F.,(4,2,2,2,4),(0.221433756193333,
0.25700303103906,0.305034737264906,0.367792942572609,0.368304303463133),
 .UNSPECIFIED.);
#353=B_SPLINE_CURVE_WITH_KNOTS('',3,(#10792,#10793,#10794,#10795,#10796,
#10797,#10798,#10799,#10800,#10801),.UNSPECIFIED.,.F.,.F.,(4,2,2,2,4),(-0.178698063530463,
-0.135269559355353,-0.0766249801953056,0.,0.000624348926771406),
 .UNSPECIFIED.);
#354=B_SPLINE_CURVE_WITH_KNOTS('',3,(#10802,#10803,#10804,#10805,#10806,
#10807,#10808,#10809,#10810,#10811),.UNSPECIFIED.,.F.,.F.,(4,2,2,2,4),(0.221433756193692,
0.2570030310401,0.30503473726647,0.367792942548679,0.368304303439319),
 .UNSPECIFIED.);
#355=B_SPLINE_CURVE_WITH_KNOTS('',3,(#10813,#10814,#10815,#10816,#10817,
#10818,#10819,#10820,#10821,#10822),.UNSPECIFIED.,.F.,.F.,(4,2,2,2,4),(-0.178698063395802,
-0.135269559262804,-0.0766249801587596,0.,0.00062434892634055),
 .UNSPECIFIED.);
#356=B_SPLINE_CURVE_WITH_KNOTS('',3,(#10824,#10825,#10826,#10827,#10828,
#10829,#10830,#10831,#10832,#10833),.UNSPECIFIED.,.F.,.F.,(4,2,2,2,4),(0.221433756192834,
0.257003031038388,0.305034737264263,0.367792942576978,0.368304303467952),
 .UNSPECIFIED.);
#357=B_SPLINE_CURVE_WITH_KNOTS('',3,(#10853,#10854,#10855,#10856,#10857,
#10858,#10859,#10860),.UNSPECIFIED.,.F.,.F.,(4,2,2,4),(-1.01270550863141,
-0.972225883052009,-0.93592471729076,-0.9302261633243),.UNSPECIFIED.);
#358=B_SPLINE_CURVE_WITH_KNOTS('',3,(#10862,#10863,#10864,#10865,#10866,
#10867,#10868,#10869,#10870,#10871,#10872,#10873,#10874,#10875,#10876,#10877,
#10878,#10879,#10880,#10881,#10882,#10883),.UNSPECIFIED.,.F.,.F.,(4,2,2,
2,2,2,2,2,2,2,4),(0.770301299294677,0.776837516381544,0.810179859704117,
0.863854547164407,0.965601485426607,1.16658222290299,1.71041595764289,2.04547866914785,
2.21675572625692,2.31744906128486,2.32707423972487),.UNSPECIFIED.);
#359=B_SPLINE_CURVE_WITH_KNOTS('',3,(#10889,#10890,#10891,#10892,#10893,
#10894,#10895,#10896,#10897,#10898,#10899,#10900,#10901,#10902,#10903,#10904,
#10905,#10906,#10907,#10908,#10909,#10910,#10911,#10912,#10913),
 .UNSPECIFIED.,.F.,.F.,(4,2,2,2,2,3,2,2,2,2,2,4),(-0.9302261633243,-0.897559179923855,
-0.841033612998941,-0.72014052841894,-0.534875041413907,0.,0.287237711284631,
0.543909079429507,0.657892073847931,0.715678915934471,0.748705009105826,
0.770301299294677),.UNSPECIFIED.);
#360=B_SPLINE_CURVE_WITH_KNOTS('',3,(#10947,#10948,#10949,#10950,#10951,
#10952,#10953,#10954,#10955,#10956,#10957,#10958,#10959,#10960,#10961,#10962,
#10963,#10964,#10965,#10966,#10967,#10968,#10969,#10970,#10971,#10972,#10973,
#10974,#10975,#10976,#10977,#10978,#10979,#10980,#10981,#10982,#10983,#10984,
#10985,#10986,#10987,#10988,#10989,#10990),.UNSPECIFIED.,.T.,.F.,(4,2,2,
2,2,2,2,2,2,2,2,2,2,2,2,2,2,2,2,2,2,4),(-3.33977974833692,-3.05254203705232,
-2.79587066890727,-2.68188767448872,-2.62410083240212,-2.59107473923068,
-2.56294223195498,-2.52959988863245,-2.47592520117237,-2.37417826291126,
-2.17319752543706,-1.62936379070288,-1.29430107920164,-1.12302402209434,
-1.02233068706724,-0.972225883048282,-0.935924717287512,-0.897559179921191,
-0.841033612997187,-0.720140528418584,-0.534875041413949,0.),
 .UNSPECIFIED.);
#361=B_SPLINE_CURVE_WITH_KNOTS('',3,(#10992,#10993,#10994,#10995,#10996,
#10997,#10998,#10999,#11000,#11001,#11002,#11003,#11004,#11005,#11006,#11007,
#11008,#11009,#11010,#11011,#11012,#11013,#11014,#11015,#11016,#11017,#11018,
#11019,#11020,#11021,#11022,#11023,#11024,#11025,#11026,#11027,#11028,#11029,
#11030,#11031,#11032,#11033,#11034,#11035),.UNSPECIFIED.,.T.,.F.,(4,2,2,
2,2,2,2,2,2,2,2,2,2,2,2,2,2,2,2,2,2,4),(-3.3397797483622,-3.05254203707762,
-2.79587066893242,-2.68188767451365,-2.62410083242683,-2.5910747392553,
-2.5629422319795,-2.52959988865681,-2.47592520119621,-2.37417826293345,
-2.17319752545607,-1.62936379071395,-1.29430107920719,-1.1230240220981,
-1.02233068707054,-0.972225883051298,-0.93592471729009,-0.89755917992317,
-0.841033612998203,-0.720140528418294,-0.534875041413579,0.),
 .UNSPECIFIED.);
#362=B_SPLINE_CURVE_WITH_KNOTS('',3,(#11037,#11038,#11039,#11040,#11041,
#11042,#11043,#11044,#11045,#11046,#11047,#11048,#11049,#11050,#11051,#11052,
#11053,#11054,#11055,#11056,#11057,#11058,#11059,#11060,#11061,#11062,#11063,
#11064,#11065,#11066,#11067,#11068,#11069,#11070,#11071,#11072,#11073,#11074,
#11075,#11076,#11077,#11078,#11079,#11080),.UNSPECIFIED.,.T.,.F.,(4,2,2,
2,2,2,2,2,2,2,2,2,2,2,2,2,2,2,2,2,2,4),(-3.3397797483903,-3.05254203710569,
-2.79587066896086,-2.68188767454252,-2.62410083245608,-2.59107473928483,
-2.56294223200934,-2.52959988868709,-2.47592520122646,-2.37417826296174,
-2.17319752548078,-1.62936379072977,-1.29430107921846,-1.12302402210607,
-1.02233068707609,-0.972225883055856,-0.935924717293985,-0.897559179926439,
-0.841033613000712,-0.720140528419696,-0.534875041414283,0.),
 .UNSPECIFIED.);
#363=B_SPLINE_CURVE_WITH_KNOTS('',3,(#11156,#11157,#11158,#11159,#11160,
#11161),.UNSPECIFIED.,.F.,.F.,(4,2,4),(0.661047189651573,0.682893822496354,
0.69260663288377),.UNSPECIFIED.);
#364=B_SPLINE_CURVE_WITH_KNOTS('',3,(#11165,#11166,#11167,#11168,#11169,
#11170),.UNSPECIFIED.,.F.,.F.,(4,2,4),(0.954385955540414,0.955688960187291,
0.983990255335198),.UNSPECIFIED.);
#365=B_SPLINE_CURVE_WITH_KNOTS('',3,(#11174,#11175,#11176,#11177,#11178,
#11179),.UNSPECIFIED.,.F.,.F.,(4,2,4),(0.11431583352954,0.135832218753253,
0.145774815807224),.UNSPECIFIED.);
#366=B_SPLINE_CURVE_WITH_KNOTS('',3,(#11182,#11183,#11184,#11185,#11186,
#11187),.UNSPECIFIED.,.F.,.F.,(4,2,4),(0.406957049146252,0.408029153839697,
0.43652027355868),.UNSPECIFIED.);
#367=B_SPLINE_CURVE_WITH_KNOTS('',3,(#11193,#11194,#11195,#11196,#11197,
#11198,#11199,#11200,#11201,#11202),.UNSPECIFIED.,.F.,.F.,(4,2,2,2,4),(-0.178698063821344,
-0.13526955955559,-0.076624980274606,0.,0.000624348927189005),
 .UNSPECIFIED.);
#368=B_SPLINE_CURVE_WITH_KNOTS('',3,(#11203,#11204,#11205,#11206,#11207,
#11208,#11209,#11210,#11211,#11212),.UNSPECIFIED.,.F.,.F.,(4,2,2,2,4),(0.221433756193381,
0.257003031040665,0.305034737267452,0.367792942517405,0.3683043034075),
 .UNSPECIFIED.);
#369=B_SPLINE_CURVE_WITH_KNOTS('',3,(#11214,#11215,#11216,#11217,#11218,
#11219,#11220,#11221,#11222,#11223),.UNSPECIFIED.,.F.,.F.,(4,2,2,2,4),(-0.178698063657826,
-0.135269559443281,-0.0766249802302674,0.,0.000624348926984052),
 .UNSPECIFIED.);
#370=B_SPLINE_CURVE_WITH_KNOTS('',3,(#11225,#11226,#11227,#11228,#11229,
#11230,#11231,#11232,#11233,#11234),.UNSPECIFIED.,.F.,.F.,(4,2,2,2,4),(0.22143375619356,
0.257003031040236,0.305034737266783,0.367792942534155,0.36830430342492),
 .UNSPECIFIED.);
#371=B_SPLINE_CURVE_WITH_KNOTS('',3,(#11241,#11242,#11243,#11244,#11245,
#11246),.UNSPECIFIED.,.F.,.F.,(4,2,4),(0.661047189631137,0.682893822475484,
0.692606632862655),.UNSPECIFIED.);
#372=B_SPLINE_CURVE_WITH_KNOTS('',3,(#11250,#11251,#11252,#11253,#11254,
#11255),.UNSPECIFIED.,.F.,.F.,(4,2,4),(0.954385955875588,0.955688960523108,
0.983990255684603),.UNSPECIFIED.);
#373=B_SPLINE_CURVE_WITH_KNOTS('',3,(#11259,#11260,#11261,#11262,#11263,
#11264),.UNSPECIFIED.,.F.,.F.,(4,2,4),(0.11431583355748,0.135832218786672,
0.145774815843186),.UNSPECIFIED.);
#374=B_SPLINE_CURVE_WITH_KNOTS('',3,(#11267,#11268,#11269,#11270,#11271,
#11272),.UNSPECIFIED.,.F.,.F.,(4,2,4),(0.406957049130622,0.408029153824045,
0.436520273542523),.UNSPECIFIED.);
#375=B_SPLINE_CURVE_WITH_KNOTS('',3,(#11282,#11283,#11284,#11285,#11286,
#11287),.UNSPECIFIED.,.F.,.F.,(4,2,4),(0.661047189621191,0.682893822464398,
0.692606632851314),.UNSPECIFIED.);
#376=B_SPLINE_CURVE_WITH_KNOTS('',3,(#11291,#11292,#11293,#11294,#11295,
#11296),.UNSPECIFIED.,.F.,.F.,(4,2,4),(0.954385955650832,0.95568896029806,
0.983990255452134),.UNSPECIFIED.);
#377=B_SPLINE_CURVE_WITH_KNOTS('',3,(#11300,#11301,#11302,#11303,#11304,
#11305),.UNSPECIFIED.,.F.,.F.,(4,2,4),(0.114315833531678,0.135832218756235,
0.145774815810657),.UNSPECIFIED.);
#378=B_SPLINE_CURVE_WITH_KNOTS('',3,(#11308,#11309,#11310,#11311,#11312,
#11313),.UNSPECIFIED.,.F.,.F.,(4,2,4),(0.406957049123385,0.408029153816832,
0.43652027353595),.UNSPECIFIED.);
#379=B_SPLINE_CURVE_WITH_KNOTS('',3,(#11323,#11324,#11325,#11326,#11327,
#11328),.UNSPECIFIED.,.F.,.F.,(4,2,4),(0.661047189700789,0.682893822549002,
0.692606632937976),.UNSPECIFIED.);
#380=B_SPLINE_CURVE_WITH_KNOTS('',3,(#11332,#11333,#11334,#11335,#11336,
#11337),.UNSPECIFIED.,.F.,.F.,(4,2,4),(0.954385955972242,0.955688960619816,
0.983990255786846),.UNSPECIFIED.);
#381=B_SPLINE_CURVE_WITH_KNOTS('',3,(#11341,#11342,#11343,#11344,#11345,
#11346),.UNSPECIFIED.,.F.,.F.,(4,2,4),(0.114315833560946,0.135832218791008,
0.145774815847966),.UNSPECIFIED.);
#382=B_SPLINE_CURVE_WITH_KNOTS('',3,(#11349,#11350,#11351,#11352,#11353,
#11354),.UNSPECIFIED.,.F.,.F.,(4,2,4),(0.406957049170082,0.408029153863569,
0.436520273584039),.UNSPECIFIED.);
#383=B_SPLINE_CURVE_WITH_KNOTS('',3,(#11360,#11361,#11362,#11363,#11364,
#11365,#11366,#11367,#11368,#11369),.UNSPECIFIED.,.F.,.F.,(4,2,2,2,4),(-0.17869806353704,
-0.135269559359834,-0.0766249801970823,0.,0.000624348926732177),
 .UNSPECIFIED.);
#384=B_SPLINE_CURVE_WITH_KNOTS('',3,(#11370,#11371,#11372,#11373,#11374,
#11375,#11376,#11377,#11378,#11379),.UNSPECIFIED.,.F.,.F.,(4,2,2,2,4),(0.221433756192697,
0.257003031038445,0.305034737264325,0.3677929425703,0.368304303461073),
 .UNSPECIFIED.);
#385=B_SPLINE_CURVE_WITH_KNOTS('',3,(#11381,#11382,#11383,#11384,#11385,
#11386,#11387,#11388,#11389,#11390),.UNSPECIFIED.,.F.,.F.,(4,2,2,2,4),(-0.178698063770044,
-0.135269559520182,-0.0766249802604931,0.,0.000624348926843672),
 .UNSPECIFIED.);
#386=B_SPLINE_CURVE_WITH_KNOTS('',3,(#11392,#11393,#11394,#11395,#11396,
#11397,#11398,#11399,#11400,#11401),.UNSPECIFIED.,.F.,.F.,(4,2,2,2,4),(0.221433756193478,
0.257003031040149,0.305034737266569,0.367792942538401,0.368304303428461),
 .UNSPECIFIED.);
#387=B_SPLINE_CURVE_WITH_KNOTS('',3,(#11404,#11405,#11406,#11407,#11408,
#11409,#11410,#11411,#11412,#11413),.UNSPECIFIED.,.F.,.F.,(4,2,2,2,4),(-0.178698063553284,
-0.135269559371072,-0.0766249802015666,0.,0.000624348926677296),
 .UNSPECIFIED.);
#388=B_SPLINE_CURVE_WITH_KNOTS('',3,(#11414,#11415,#11416,#11417,#11418,
#11419,#11420,#11421,#11422,#11423),.UNSPECIFIED.,.F.,.F.,(4,2,2,2,4),(0.221433756192838,
0.25700303103897,0.305034737265084,0.367792942555533,0.368304303445851),
 .UNSPECIFIED.);
#389=B_SPLINE_CURVE_WITH_KNOTS('',3,(#11425,#11426,#11427,#11428,#11429,
#11430,#11431,#11432,#11433,#11434),.UNSPECIFIED.,.F.,.F.,(4,2,2,2,4),(-0.178698063553173,
-0.135269559370956,-0.0766249802014978,0.,0.000624348926817562),
 .UNSPECIFIED.);
#390=B_SPLINE_CURVE_WITH_KNOTS('',3,(#11436,#11437,#11438,#11439,#11440,
#11441,#11442,#11443,#11444,#11445),.UNSPECIFIED.,.F.,.F.,(4,2,2,2,4),(0.221433756193333,
0.25700303103906,0.305034737264906,0.367792942572609,0.368304303463133),
 .UNSPECIFIED.);
#391=B_SPLINE_CURVE_WITH_KNOTS('',3,(#11448,#11449,#11450,#11451,#11452,
#11453,#11454,#11455,#11456,#11457),.UNSPECIFIED.,.F.,.F.,(4,2,2,2,4),(-0.178698063530463,
-0.135269559355353,-0.0766249801953056,0.,0.000624348926771406),
 .UNSPECIFIED.);
#392=B_SPLINE_CURVE_WITH_KNOTS('',3,(#11458,#11459,#11460,#11461,#11462,
#11463,#11464,#11465,#11466,#11467),.UNSPECIFIED.,.F.,.F.,(4,2,2,2,4),(0.221433756193692,
0.2570030310401,0.30503473726647,0.367792942548679,0.368304303439319),
 .UNSPECIFIED.);
#393=B_SPLINE_CURVE_WITH_KNOTS('',3,(#11469,#11470,#11471,#11472,#11473,
#11474,#11475,#11476,#11477,#11478),.UNSPECIFIED.,.F.,.F.,(4,2,2,2,4),(-0.178698063395802,
-0.135269559262804,-0.0766249801587596,0.,0.00062434892634055),
 .UNSPECIFIED.);
#394=B_SPLINE_CURVE_WITH_KNOTS('',3,(#11480,#11481,#11482,#11483,#11484,
#11485,#11486,#11487,#11488,#11489),.UNSPECIFIED.,.F.,.F.,(4,2,2,2,4),(0.221433756192834,
0.257003031038388,0.305034737264263,0.367792942576978,0.368304303467952),
 .UNSPECIFIED.);
#395=B_SPLINE_CURVE_WITH_KNOTS('',3,(#11718,#11719,#11720,#11721,#11722,
#11723,#11724,#11725,#11726,#11727,#11728,#11729,#11730,#11731),
 .UNSPECIFIED.,.F.,.F.,(4,2,2,2,2,2,4),(9.25473526333439,9.54447442505159,
9.8342135867688,10.4136919102032,10.9910554946856,11.2797372869268,11.568419079168),
 .UNSPECIFIED.);
#396=B_SPLINE_CURVE_WITH_KNOTS('',3,(#11733,#11734,#11735,#11736,#11737,
#11738,#11739,#11740,#11741,#11742,#11743,#11744,#11745,#11746),
 .UNSPECIFIED.,.F.,.F.,(4,2,2,2,2,2,4),(6.94105144750079,7.22973323974199,
7.51841503198319,8.09577861646558,8.67525693989999,8.96499610161719,9.25473526333439),
 .UNSPECIFIED.);
#397=B_SPLINE_CURVE_WITH_KNOTS('',3,(#11751,#11752,#11753,#11754,#11755,
#11756,#11757,#11758,#11759,#11760,#11761,#11762,#11763,#11764),
 .UNSPECIFIED.,.F.,.F.,(4,2,2,2,2,2,4),(4.6273676316672,4.9171067933844,
5.2068459551016,5.78632427853601,6.3636878630184,6.6523696552596,6.94105144750079),
 .UNSPECIFIED.);
#398=B_SPLINE_CURVE_WITH_KNOTS('',3,(#11765,#11766,#11767,#11768,#11769,
#11770,#11771,#11772,#11773,#11774,#11775,#11776,#11777,#11778),
 .UNSPECIFIED.,.F.,.F.,(4,2,2,2,2,2,4),(11.568419079168,11.8571008714092,
12.1457826636504,12.7231462481328,13.3026245715672,13.5923637332844,13.8821028950016),
 .UNSPECIFIED.);
#399=B_SPLINE_CURVE_WITH_KNOTS('',3,(#11781,#11782,#11783,#11784,#11785,
#11786,#11787,#11788,#11789,#11790,#11791,#11792,#11793,#11794,#11795,#11796,
#11797,#11798,#11799,#11800,#11801,#11802,#11803,#11804,#11805,#11806),
 .UNSPECIFIED.,.F.,.F.,(4,2,2,2,2,2,2,2,2,2,2,2,4),(4.6273676316672,4.9171067933844,
5.2068459551016,5.78632427853601,6.3636878630184,6.6523696552596,6.94105144750079,
7.22973323974199,7.51841503198319,8.09577861646558,8.67525693989999,8.96499610161719,
9.25473526333439),.UNSPECIFIED.);
#400=B_SPLINE_CURVE_WITH_KNOTS('',3,(#11807,#11808,#11809,#11810,#11811,
#11812,#11813,#11814,#11815,#11816,#11817,#11818,#11819,#11820,#11821,#11822,
#11823,#11824,#11825,#11826,#11827,#11828,#11829,#11830,#11831,#11832),
 .UNSPECIFIED.,.F.,.F.,(4,2,2,2,2,2,2,2,2,2,2,2,4),(9.25473526333439,9.54447442505159,
9.8342135867688,10.4136919102032,10.9910554946856,11.2797372869268,11.568419079168,
11.8571008714092,12.1457826636504,12.7231462481328,13.3026245715672,13.5923637332844,
13.8821028950016),.UNSPECIFIED.);
#401=B_SPLINE_CURVE_WITH_KNOTS('',3,(#11835,#11836,#11837,#11838,#11839,
#11840,#11841,#11842,#11843,#11844,#11845,#11846,#11847,#11848,#11849,#11850,
#11851,#11852,#11853,#11854,#11855,#11856,#11857,#11858,#11859,#11860),
 .UNSPECIFIED.,.F.,.F.,(4,2,2,2,2,2,2,2,2,2,2,2,4),(4.62736763166719,4.9171067933844,
5.2068459551016,5.78632427853601,6.3636878630184,6.6523696552596,6.94105144750079,
7.22973323974199,7.51841503198319,8.09577861646558,8.67525693989998,8.96499610161719,
9.25473526333439),.UNSPECIFIED.);
#402=B_SPLINE_CURVE_WITH_KNOTS('',3,(#11861,#11862,#11863,#11864,#11865,
#11866,#11867,#11868,#11869,#11870,#11871,#11872,#11873,#11874,#11875,#11876,
#11877,#11878,#11879,#11880,#11881,#11882,#11883,#11884,#11885,#11886),
 .UNSPECIFIED.,.F.,.F.,(4,2,2,2,2,2,2,2,2,2,2,2,4),(9.25473526333439,9.54447442505159,
9.8342135867688,10.4136919102032,10.9910554946856,11.2797372869268,11.568419079168,
11.8571008714092,12.1457826636504,12.7231462481328,13.3026245715672,13.5923637332844,
13.8821028950016),.UNSPECIFIED.);
#403=B_SPLINE_CURVE_WITH_KNOTS('',3,(#11929,#11930,#11931,#11932,#11933,
#11934,#11935,#11936,#11937,#11938,#11939,#11940,#11941,#11942),
 .UNSPECIFIED.,.F.,.F.,(4,2,2,2,2,2,4),(-4.06985486860275,-3.8142561336285,
-3.55865739865425,-3.04745992870576,-2.54119368150357,-2.28806055790247,
-2.03492743430138),.UNSPECIFIED.);
#404=B_SPLINE_CURVE_WITH_KNOTS('',3,(#11944,#11945,#11946,#11947,#11948,
#11949,#11950,#11951,#11952,#11953,#11954,#11955,#11956,#11957),
 .UNSPECIFIED.,.F.,.F.,(4,2,2,2,2,2,4),(2.03492743430138,2.28806055790247,
2.54119368150357,3.04745992870576,3.55865739865425,3.8142561336285,4.06985486860275),
 .UNSPECIFIED.);
#405=B_SPLINE_CURVE_WITH_KNOTS('',3,(#11959,#11960,#11961,#11962,#11963,
#11964,#11965,#11966,#11967,#11968,#11969,#11970,#11971,#11972),
 .UNSPECIFIED.,.F.,.F.,(4,2,2,2,2,2,4),(0.,0.255598734974248,0.511197469948496,
1.02239493989699,1.52866118709918,1.78179431070028,2.03492743430138),
 .UNSPECIFIED.);
#406=B_SPLINE_CURVE_WITH_KNOTS('',3,(#11974,#11975,#11976,#11977,#11978,
#11979,#11980,#11981,#11982,#11983,#11984,#11985,#11986,#11987),
 .UNSPECIFIED.,.F.,.F.,(4,2,2,2,2,2,4),(-2.03492743430138,-1.78179431070028,
-1.52866118709918,-1.02239493989699,-0.511197469948497,-0.255598734974249,
0.),.UNSPECIFIED.);
#407=B_SPLINE_CURVE_WITH_KNOTS('',3,(#12049,#12050,#12051,#12052,#12053,
#12054,#12055,#12056,#12057,#12058,#12059,#12060,#12061,#12062,#12063,#12064,
#12065,#12066,#12067,#12068,#12069,#12070,#12071,#12072,#12073,#12074),
 .UNSPECIFIED.,.F.,.F.,(4,2,2,2,2,2,2,2,2,2,2,2,4),(-4.06985486860275,-3.8142561336285,
-3.55865739865425,-3.04745992870576,-2.54119368150357,-2.28806055790247,
-2.03492743430138,-1.78179431070028,-1.52866118709918,-1.02239493989699,
-0.511197469948497,-0.255598734974249,0.),.UNSPECIFIED.);
#408=B_SPLINE_CURVE_WITH_KNOTS('',3,(#12075,#12076,#12077,#12078,#12079,
#12080,#12081,#12082,#12083,#12084,#12085,#12086,#12087,#12088,#12089,#12090,
#12091,#12092,#12093,#12094,#12095,#12096,#12097,#12098,#12099,#12100),
 .UNSPECIFIED.,.F.,.F.,(4,2,2,2,2,2,2,2,2,2,2,2,4),(0.,0.255598734974248,
0.511197469948495,1.02239493989699,1.52866118709918,1.78179431070028,2.03492743430137,
2.28806055790247,2.54119368150357,3.04745992870576,3.55865739865425,3.8142561336285,
4.06985486860275),.UNSPECIFIED.);
#409=B_SPLINE_CURVE_WITH_KNOTS('',3,(#12105,#12106,#12107,#12108,#12109,
#12110,#12111,#12112,#12113,#12114,#12115,#12116,#12117,#12118,#12119,#12120,
#12121,#12122,#12123,#12124,#12125,#12126,#12127,#12128,#12129,#12130),
 .UNSPECIFIED.,.F.,.F.,(4,2,2,2,2,2,2,2,2,2,2,2,4),(-4.06985486860275,-3.8142561336285,
-3.55865739865425,-3.04745992870576,-2.54119368150357,-2.28806055790247,
-2.03492743430137,-1.78179431070028,-1.52866118709918,-1.02239493989699,
-0.511197469948497,-0.255598734974249,0.),.UNSPECIFIED.);
#410=B_SPLINE_CURVE_WITH_KNOTS('',3,(#12131,#12132,#12133,#12134,#12135,
#12136,#12137,#12138,#12139,#12140,#12141,#12142,#12143,#12144,#12145,#12146,
#12147,#12148,#12149,#12150,#12151,#12152,#12153,#12154,#12155,#12156),
 .UNSPECIFIED.,.F.,.F.,(4,2,2,2,2,2,2,2,2,2,2,2,4),(0.,0.255598734974248,
0.511197469948495,1.02239493989699,1.52866118709918,1.78179431070028,2.03492743430137,
2.28806055790247,2.54119368150357,3.04745992870576,3.55865739865425,3.8142561336285,
4.06985486860275),.UNSPECIFIED.);
#411=B_SPLINE_CURVE_WITH_KNOTS('',3,(#12350,#12351,#12352,#12353,#12354,
#12355,#12356,#12357),.UNSPECIFIED.,.F.,.F.,(4,2,2,4),(0.801601659973552,
0.908686694681274,1.06147652934293,1.21426636400458),.UNSPECIFIED.);
#412=B_SPLINE_CURVE_WITH_KNOTS('',3,(#12359,#12360,#12361,#12362,#12363,
#12364,#12365,#12366,#12367,#12368,#12369,#12370,#12371,#12372),
 .UNSPECIFIED.,.F.,.F.,(4,2,2,2,2,2,4),(0.,0.152789834661652,0.305579669323305,
0.456356425662796,0.607133182002287,0.757909938341781,0.801601659973552),
 .UNSPECIFIED.);
#413=B_SPLINE_CURVE_WITH_KNOTS('',3,(#12376,#12377,#12378,#12379,#12380,
#12381,#12382,#12383,#12384,#12385,#12386,#12387,#12388,#12389,#12390,#12391),
 .UNSPECIFIED.,.F.,.F.,(4,2,2,2,2,2,2,4),(1.41258149283994,1.51470567835646,
1.66615965590029,1.81761363344413,1.96906761098797,2.12052158853181,2.27200321656199,
2.42348484459217),.UNSPECIFIED.);
#414=B_SPLINE_CURVE_WITH_KNOTS('',3,(#12392,#12393,#12394,#12395,#12396,
#12397),.UNSPECIFIED.,.F.,.F.,(4,2,4),(1.21174242229609,1.36322405032627,
1.41258149283994),.UNSPECIFIED.);
#415=B_SPLINE_CURVE_WITH_KNOTS('',3,(#12402,#12403,#12404,#12405,#12406,
#12407,#12408,#12409),.UNSPECIFIED.,.F.,.F.,(4,2,2,4),(0.810459053731311,
0.931112082660273,1.09792489409666,1.26473770553305),.UNSPECIFIED.);
#416=B_SPLINE_CURVE_WITH_KNOTS('',3,(#12411,#12412,#12413,#12414,#12415,
#12416,#12417,#12418,#12419,#12420,#12421,#12422,#12423,#12424),
 .UNSPECIFIED.,.F.,.F.,(4,2,2,2,2,2,4),(0.,0.166812811436392,0.333625622872784,
0.482997237819655,0.632368852766526,0.781740467713401,0.810459053731311),
 .UNSPECIFIED.);
#417=B_SPLINE_CURVE_WITH_KNOTS('',3,(#12426,#12427,#12428,#12429,#12430,
#12431,#12432,#12433,#12434,#12435,#12436,#12437,#12438,#12439,#12440,#12441,
#12442,#12443),.UNSPECIFIED.,.F.,.F.,(4,2,2,2,2,2,2,2,4),(1.21426636400458,
1.37281902636882,1.53137168873306,1.68587949128402,1.84038729383497,1.99489509638593,
2.14940289893689,2.30795556130114,2.46650822366539),.UNSPECIFIED.);
#418=B_SPLINE_CURVE_WITH_KNOTS('',3,(#12448,#12449,#12450,#12451,#12452,
#12453,#12454,#12455,#12456,#12457),.UNSPECIFIED.,.F.,.F.,(4,2,2,2,4),(0.84921255840186,
0.855460999411689,1.0133776521287,1.20423317275903,1.39508869338936),
 .UNSPECIFIED.);
#419=B_SPLINE_CURVE_WITH_KNOTS('',3,(#12459,#12460,#12461,#12462,#12463,
#12464,#12465,#12466,#12467,#12468,#12469,#12470),.UNSPECIFIED.,.F.,.F.,
(4,2,2,2,2,4),(0.,0.19085552063033,0.38171104126066,0.539627693977667,0.697544346694674,
0.84921255840186),.UNSPECIFIED.);
#420=B_SPLINE_CURVE_WITH_KNOTS('',3,(#12472,#12473,#12474,#12475,#12476,
#12477,#12478,#12479,#12480,#12481,#12482,#12483,#12484,#12485,#12486,#12487,
#12488,#12489),.UNSPECIFIED.,.F.,.F.,(4,2,2,2,2,2,2,2,4),(1.26473770553305,
1.44115993597425,1.61758216641546,1.77878219205947,1.93998221770349,2.10118224334752,
2.26238226899155,2.43880449943275,2.61522672987395),.UNSPECIFIED.);
#421=B_SPLINE_CURVE_WITH_KNOTS('',3,(#12493,#12494,#12495,#12496,#12497,
#12498,#12499,#12500,#12501,#12502,#12503,#12504,#12505,#12506,#12507,#12508,
#12509,#12510,#12511,#12512,#12513,#12514),.UNSPECIFIED.,.F.,.F.,(4,2,2,
2,2,2,2,2,2,2,4),(1.39508869338936,1.63068735474474,1.86628601610013,2.01895939966093,
2.09529609144134,2.17163278322174,2.24796947500215,2.32430616678255,2.47697955034337,
2.71257821169876,2.94817687305416),.UNSPECIFIED.);
#422=B_SPLINE_CURVE_WITH_KNOTS('',3,(#12517,#12518,#12519,#12520,#12521,
#12522,#12523,#12524,#12525,#12526,#12527,#12528,#12529,#12530,#12531,#12532,
#12533,#12534,#12535,#12536,#12537,#12538,#12539,#12540,#12541,#12542),
 .UNSPECIFIED.,.F.,.F.,(4,2,2,2,2,2,2,2,2,2,2,2,4),(0.,0.0444658256706816,
0.109825747467382,0.210987273969983,0.363115011869221,0.476603266918211,
0.543343022865724,0.610052308554092,0.7232875236507,0.87579543247345,0.97697424211648,
1.04237097445545,1.08685368328188),.UNSPECIFIED.);
#423=B_SPLINE_CURVE_WITH_KNOTS('',3,(#12557,#12558,#12559,#12560,#12561,
#12562,#12563,#12564),.UNSPECIFIED.,.F.,.F.,(4,2,2,4),(0.801601659973551,
0.908686694681269,1.06147652934292,1.21426636400457),.UNSPECIFIED.);
#424=B_SPLINE_CURVE_WITH_KNOTS('',3,(#12566,#12567,#12568,#12569,#12570,
#12571,#12572,#12573,#12574,#12575,#12576,#12577,#12578,#12579),
 .UNSPECIFIED.,.F.,.F.,(4,2,2,2,2,2,4),(0.,0.152789834661651,0.305579669323302,
0.456356425662796,0.607133182002289,0.757909938341779,0.801601659973551),
 .UNSPECIFIED.);
#425=B_SPLINE_CURVE_WITH_KNOTS('',3,(#12583,#12584,#12585,#12586,#12587,
#12588,#12589,#12590,#12591,#12592,#12593,#12594,#12595,#12596,#12597,#12598),
 .UNSPECIFIED.,.F.,.F.,(4,2,2,2,2,2,2,4),(1.41258149283993,1.51470567835645,
1.66615965590029,1.81761363344413,1.96906761098797,2.1205215885318,2.27200321656199,
2.42348484459217),.UNSPECIFIED.);
#426=B_SPLINE_CURVE_WITH_KNOTS('',3,(#12599,#12600,#12601,#12602,#12603,
#12604),.UNSPECIFIED.,.F.,.F.,(4,2,4),(1.21174242229609,1.36322405032627,
1.41258149283993),.UNSPECIFIED.);
#427=B_SPLINE_CURVE_WITH_KNOTS('',3,(#12609,#12610,#12611,#12612,#12613,
#12614,#12615,#12616),.UNSPECIFIED.,.F.,.F.,(4,2,2,4),(0.810459053731318,
0.931112082660271,1.09792489409666,1.26473770553306),.UNSPECIFIED.);
#428=B_SPLINE_CURVE_WITH_KNOTS('',3,(#12618,#12619,#12620,#12621,#12622,
#12623,#12624,#12625,#12626,#12627,#12628,#12629,#12630,#12631),
 .UNSPECIFIED.,.F.,.F.,(4,2,2,2,2,2,4),(0.,0.166812811436393,0.333625622872785,
0.482997237819654,0.632368852766523,0.781740467713397,0.810459053731318),
 .UNSPECIFIED.);
#429=B_SPLINE_CURVE_WITH_KNOTS('',3,(#12633,#12634,#12635,#12636,#12637,
#12638,#12639,#12640,#12641,#12642,#12643,#12644,#12645,#12646,#12647,#12648,
#12649,#12650),.UNSPECIFIED.,.F.,.F.,(4,2,2,2,2,2,2,2,4),(1.21426636400457,
1.37281902636881,1.53137168873306,1.68587949128401,1.84038729383497,1.99489509638593,
2.14940289893689,2.30795556130114,2.46650822366538),.UNSPECIFIED.);
#430=B_SPLINE_CURVE_WITH_KNOTS('',3,(#12655,#12656,#12657,#12658,#12659,
#12660,#12661,#12662),.UNSPECIFIED.,.F.,.F.,(4,2,2,4),(0.848478832255458,
0.991796836691898,1.19347267089766,1.39514850510343),.UNSPECIFIED.);
#431=B_SPLINE_CURVE_WITH_KNOTS('',3,(#12664,#12665,#12666,#12667,#12668,
#12669,#12670,#12671,#12672,#12673,#12674,#12675,#12676,#12677),
 .UNSPECIFIED.,.F.,.F.,(4,2,2,2,2,2,4),(0.,0.201675834205757,0.403351668411514,
0.550462960481608,0.697574252551703,0.8446855446218,0.848478832255458),
 .UNSPECIFIED.);
#432=B_SPLINE_CURVE_WITH_KNOTS('',3,(#12679,#12680,#12681,#12682,#12683,
#12684,#12685,#12686,#12687,#12688,#12689,#12690,#12691,#12692,#12693,#12694,
#12695,#12696),.UNSPECIFIED.,.F.,.F.,(4,2,2,2,2,2,2,2,4),(1.26473770553306,
1.44115993597426,1.61758216641546,1.77878219205948,1.93998221770349,2.10118224334752,
2.26238226899154,2.43880449943275,2.61522672987395),.UNSPECIFIED.);
#433=B_SPLINE_CURVE_WITH_KNOTS('',3,(#12700,#12701,#12702,#12703,#12704,
#12705,#12706,#12707,#12708,#12709,#12710,#12711,#12712,#12713,#12714,#12715,
#12716,#12717,#12718,#12719,#12720,#12721),.UNSPECIFIED.,.F.,.F.,(4,2,2,
2,2,2,2,2,2,2,4),(1.39514850510343,1.60860320712188,1.82205790914033,1.99791237111712,
2.08583960210551,2.17376683309391,2.26169406408231,2.34962129507071,2.5254757570475,
2.73893045906596,2.95238516108442),.UNSPECIFIED.);
#434=B_SPLINE_CURVE_WITH_KNOTS('',3,(#12724,#12725,#12726,#12727,#12728,
#12729,#12730,#12731,#12732,#12733,#12734,#12735,#12736,#12737,#12738,#12739,
#12740,#12741,#12742,#12743,#12744,#12745,#12746,#12747,#12748,#12749),
 .UNSPECIFIED.,.F.,.F.,(4,2,2,2,2,2,2,2,2,2,2,2,4),(0.,0.0444658256707017,
0.109825747467453,0.210987273970143,0.363115011869592,0.4766032669186,0.543343022866364,
0.610052308555067,0.723287523653244,0.875795432478097,0.97697424212264,
1.04237097446268,1.08685368328966),.UNSPECIFIED.);
#435=B_SPLINE_CURVE_WITH_KNOTS('',3,(#12755,#12756,#12757,#12758,#12759,
#12760,#12761,#12762),.UNSPECIFIED.,.F.,.F.,(4,2,2,4),(0.80160165997355,
0.908686694681275,1.06147652934293,1.21426636400458),.UNSPECIFIED.);
#436=B_SPLINE_CURVE_WITH_KNOTS('',3,(#12764,#12765,#12766,#12767,#12768,
#12769,#12770,#12771,#12772,#12773,#12774,#12775,#12776,#12777),
 .UNSPECIFIED.,.F.,.F.,(4,2,2,2,2,2,4),(0.,0.152789834661653,0.305579669323305,
0.456356425662799,0.607133182002292,0.757909938341784,0.80160165997355),
 .UNSPECIFIED.);
#437=B_SPLINE_CURVE_WITH_KNOTS('',3,(#12781,#12782,#12783,#12784,#12785,
#12786,#12787,#12788,#12789,#12790,#12791,#12792,#12793,#12794,#12795,#12796),
 .UNSPECIFIED.,.F.,.F.,(4,2,2,2,2,2,2,4),(1.41258149283993,1.51470567835645,
1.66615965590029,1.81761363344413,1.96906761098797,2.12052158853181,2.27200321656199,
2.42348484459217),.UNSPECIFIED.);
#438=B_SPLINE_CURVE_WITH_KNOTS('',3,(#12797,#12798,#12799,#12800,#12801,
#12802),.UNSPECIFIED.,.F.,.F.,(4,2,4),(1.21174242229609,1.36322405032627,
1.41258149283993),.UNSPECIFIED.);
#439=B_SPLINE_CURVE_WITH_KNOTS('',3,(#12807,#12808,#12809,#12810,#12811,
#12812,#12813,#12814),.UNSPECIFIED.,.F.,.F.,(4,2,2,4),(0.810451797988797,
0.931104826917751,1.09791763835414,1.26473044979053),.UNSPECIFIED.);
#440=B_SPLINE_CURVE_WITH_KNOTS('',3,(#12816,#12817,#12818,#12819,#12820,
#12821,#12822,#12823,#12824,#12825,#12826,#12827,#12828,#12829),
 .UNSPECIFIED.,.F.,.F.,(4,2,2,2,2,2,4),(0.,0.163827053405726,0.327654106811452,
0.48000785191773,0.632361597024009,0.781733211970881,0.810451797988797),
 .UNSPECIFIED.);
#441=B_SPLINE_CURVE_WITH_KNOTS('',3,(#12831,#12832,#12833,#12834,#12835,
#12836,#12837,#12838,#12839,#12840,#12841,#12842,#12843,#12844,#12845,#12846,
#12847,#12848),.UNSPECIFIED.,.F.,.F.,(4,2,2,2,2,2,2,2,4),(1.21426636400458,
1.37281902636882,1.53137168873306,1.68587949128402,1.84038729383497,1.99489509638594,
2.1494028989369,2.30795556130114,2.46650822366539),.UNSPECIFIED.);
#442=B_SPLINE_CURVE_WITH_KNOTS('',3,(#12853,#12854,#12855,#12856,#12857,
#12858,#12859,#12860,#12861,#12862),.UNSPECIFIED.,.F.,.F.,(4,2,2,2,4),(0.849212558401863,
0.855460999411694,1.01337765212871,1.20423317275904,1.39508869338936),
 .UNSPECIFIED.);
#443=B_SPLINE_CURVE_WITH_KNOTS('',3,(#12864,#12865,#12866,#12867,#12868,
#12869,#12870,#12871,#12872,#12873,#12874,#12875),.UNSPECIFIED.,.F.,.F.,
(4,2,2,2,2,4),(0.,0.190855520630331,0.381711041260663,0.539627693977671,
0.697544346694678,0.849212558401863),.UNSPECIFIED.);
#444=B_SPLINE_CURVE_WITH_KNOTS('',3,(#12877,#12878,#12879,#12880,#12881,
#12882,#12883,#12884,#12885,#12886,#12887,#12888,#12889,#12890,#12891,#12892,
#12893,#12894),.UNSPECIFIED.,.F.,.F.,(4,2,2,2,2,2,2,2,4),(1.26473044979053,
1.45047293867533,1.63621542756013,1.78793284105988,1.93965025455964,2.0913676680594,
2.24308508155916,2.42882757044396,2.61457005932877),.UNSPECIFIED.);
#445=B_SPLINE_CURVE_WITH_KNOTS('',3,(#12898,#12899,#12900,#12901,#12902,
#12903,#12904,#12905,#12906,#12907,#12908,#12909,#12910,#12911,#12912,#12913,
#12914,#12915,#12916,#12917,#12918,#12919),.UNSPECIFIED.,.F.,.F.,(4,2,2,
2,2,2,2,2,2,2,4),(1.39508869338936,1.63068735474475,1.86628601610013,2.01895939966094,
2.09529609144135,2.17163278322175,2.24796947500216,2.32430616678257,2.47697955034339,
2.71257821169878,2.94817687305417),.UNSPECIFIED.);
#446=B_SPLINE_CURVE_WITH_KNOTS('',3,(#12922,#12923,#12924,#12925,#12926,
#12927,#12928,#12929,#12930,#12931,#12932,#12933,#12934,#12935,#12936,#12937,
#12938,#12939,#12940,#12941,#12942,#12943,#12944,#12945,#12946,#12947),
 .UNSPECIFIED.,.F.,.F.,(4,2,2,2,2,2,2,2,2,2,2,2,4),(0.,0.0444658256707104,
0.109825747467599,0.210987273970278,0.3631150118696,0.476603266918339,0.54334302286555,
0.610052308553677,0.723287523650531,0.875795432473984,0.97697424211741,
1.0423709744566,1.08685368328313),.UNSPECIFIED.);
#447=B_SPLINE_CURVE_WITH_KNOTS('',3,(#13048,#13049,#13050,#13051,#13052,
#13053,#13054,#13055,#13056,#13057,#13058,#13059,#13060,#13061,#13062,#13063,
#13064,#13065),.UNSPECIFIED.,.F.,.F.,(4,2,2,2,2,2,2,2,4),(-2.42440986895006,
-2.27286833474306,-2.12132680053607,-1.9698171011243,-1.81830740171254,
-1.66679770230078,-1.51528800288901,-1.36374646868202,-1.21220493447502),
 .UNSPECIFIED.);
#448=B_SPLINE_CURVE_WITH_KNOTS('',3,(#13115,#13116,#13117,#13118,#13119,
#13120,#13121,#13122,#13123,#13124,#13125,#13126,#13127,#13128,#13129,#13130,
#13131,#13132,#13133,#13134,#13135),.UNSPECIFIED.,.F.,.F.,(4,2,2,2,3,2,
2,2,2,4),(1.63431795680218,1.63484051213071,1.74655213492763,1.90358589296679,
2.06061965100595,2.19559646985844,2.33057328871092,2.44200600177385,2.55343871483678,
2.66004451397958),.UNSPECIFIED.);
#449=B_SPLINE_CURVE_WITH_KNOTS('',3,(#13136,#13137,#13138,#13139,#13140,
#13141,#13142,#13143,#13144,#13145,#13146,#13147,#13148,#13149,#13150,#13151,
#13152,#13153,#13154,#13155,#13156,#13157,#13158,#13159),.UNSPECIFIED.,
 .F.,.F.,(4,2,2,2,2,2,2,2,2,2,2,4),(2.66004451397958,2.66487142789972,2.77630414096266,
2.91128095981515,3.04625777866764,3.20329153670679,3.36032529474595,3.47203691754285,
3.5278927289413,3.58374854033975,3.63960435173821,3.69493760780813),
 .UNSPECIFIED.);
#450=B_SPLINE_CURVE_WITH_KNOTS('',3,(#13162,#13163,#13164,#13165,#13166,
#13167,#13168,#13169,#13170,#13171,#13172,#13173,#13174,#13175,#13176,#13177,
#13178,#13179,#13180,#13181,#13182,#13183,#13184),.UNSPECIFIED.,.F.,.F.,
(4,2,2,2,3,2,2,2,2,2,4),(1.63645246149242,1.6458071028209,1.76735674157733,
1.91500283165642,2.06264892173552,2.21065304350676,2.35865716527801,2.45711954510512,
2.55558192493224,2.65404430475936,2.66124396153498),.UNSPECIFIED.);
#451=B_SPLINE_CURVE_WITH_KNOTS('',3,(#13185,#13186,#13187,#13188,#13189,
#13190,#13191,#13192,#13193,#13194,#13195,#13196,#13197,#13198,#13199,#13200,
#13201,#13202,#13203,#13204,#13205,#13206),.UNSPECIFIED.,.F.,.F.,(4,2,2,
2,2,2,2,2,2,2,4),(2.66124396153498,2.75250668458648,2.90051080635773,3.04851492812899,
3.19616101820807,3.34380710828715,3.46535674704357,3.52613156642178,3.58690638579999,
3.64768120517821,3.69910138322794),.UNSPECIFIED.);
#452=B_SPLINE_CURVE_WITH_KNOTS('',3,(#13209,#13210,#13211,#13212,#13213,
#13214,#13215,#13216,#13217,#13218,#13219,#13220,#13221,#13222,#13223,#13224,
#13225,#13226,#13227,#13228,#13229),.UNSPECIFIED.,.F.,.F.,(4,2,2,3,2,2,
2,2,2,4),(1.48658026968319,1.57668032617585,1.70181043495793,1.82694054374001,
1.94229840394621,2.0576562641524,2.16466765320846,2.27167904226452,2.37869043132058,
2.39673280800115),.UNSPECIFIED.);
#453=B_SPLINE_CURVE_WITH_KNOTS('',3,(#13230,#13231,#13232,#13233,#13234,
#13235,#13236,#13237,#13238,#13239,#13240,#13241,#13242,#13243,#13244,#13245,
#13246,#13247,#13248,#13249),.UNSPECIFIED.,.F.,.F.,(4,2,2,2,2,2,2,2,2,4),
(2.39673280800115,2.48570182037664,2.60105968058284,2.71641754078903,2.84154764957111,
2.96667775835319,3.07591353624385,3.18514931413451,3.29438509202518,3.3135208134232),
 .UNSPECIFIED.);
#454=B_SPLINE_CURVE_WITH_KNOTS('',3,(#13252,#13253,#13254,#13255,#13256,
#13257,#13258,#13259,#13260,#13261,#13262,#13263,#13264,#13265,#13266,#13267,
#13268,#13269,#13270,#13271,#13272),.UNSPECIFIED.,.F.,.F.,(4,2,2,3,2,2,
2,2,2,4),(1.48667142164751,1.57677147814025,1.70190158692234,1.82703169570442,
1.94802136665288,2.06901103760135,2.17041340390623,2.27181577021112,2.37321813651602,
2.39644556681379),.UNSPECIFIED.);
#455=B_SPLINE_CURVE_WITH_KNOTS('',3,(#13273,#13274,#13275,#13276,#13277,
#13278,#13279,#13280,#13281,#13282,#13283,#13284,#13285,#13286,#13287,#13288,
#13289,#13290,#13291,#13292),.UNSPECIFIED.,.F.,.F.,(4,2,2,2,2,2,2,2,2,4),
(2.39644556681379,2.47462050282091,2.59561017376938,2.71659984471785,2.84172995349992,
2.966860062282,3.07609584017266,3.18533161806333,3.294567395954,3.31370311735193),
 .UNSPECIFIED.);
#456=B_SPLINE_CURVE_WITH_KNOTS('',3,(#13295,#13296,#13297,#13298,#13299,
#13300,#13301,#13302,#13303,#13304,#13305,#13306,#13307,#13308,#13309,#13310,
#13311,#13312,#13313,#13314,#13315),.UNSPECIFIED.,.F.,.F.,(4,2,2,3,2,2,
2,2,2,4),(1.42510602309759,1.50257240162674,1.61295870334865,1.72334500507057,
1.83225417045197,1.94116333583337,2.04500754168813,2.1488517475429,2.25269595339766,
2.2848744256183),.UNSPECIFIED.);
#457=B_SPLINE_CURVE_WITH_KNOTS('',3,(#13316,#13317,#13318,#13319,#13320,
#13321,#13322,#13323,#13324,#13325,#13326,#13327,#13328,#13329,#13330,#13331,
#13332,#13333,#13334,#13335),.UNSPECIFIED.,.F.,.F.,(4,2,2,2,2,2,2,2,2,4),
(2.2848744256183,2.35654015925242,2.46544932463382,2.57435849001523,2.68474479173714,
2.79513109345905,2.90282767176861,3.01052425007817,3.11822082838774,3.14845102816816),
 .UNSPECIFIED.);
#458=B_SPLINE_CURVE_WITH_KNOTS('',3,(#13338,#13339,#13340,#13341,#13342,
#13343,#13344,#13345,#13346,#13347,#13348,#13349,#13350,#13351,#13352,#13353,
#13354,#13355,#13356,#13357,#13358),.UNSPECIFIED.,.F.,.F.,(4,2,2,3,2,2,
2,2,2,4),(1.42506934481542,1.50220099251643,1.61276096598296,1.72332093944948,
1.83050112648501,1.93768131352053,2.04324956210919,2.14881781069785,2.25438605928651,
2.28497277338716),.UNSPECIFIED.);
#459=B_SPLINE_CURVE_WITH_KNOTS('',3,(#13359,#13360,#13361,#13362,#13363,
#13364,#13365,#13366,#13367,#13368,#13369,#13370,#13371,#13372,#13373,#13374,
#13375,#13376,#13377,#13378),.UNSPECIFIED.,.F.,.F.,(4,2,2,2,2,2,2,2,2,4),
(2.28497277338716,2.35995430787517,2.46713449491069,2.57431468194622,2.68487465541274,
2.79543462887926,2.90295645465092,3.01047828042258,3.11800010619425,3.1483902842649),
 .UNSPECIFIED.);
#460=B_SPLINE_CURVE_WITH_KNOTS('',3,(#13381,#13382,#13383,#13384,#13385,
#13386,#13387,#13388,#13389,#13390,#13391,#13392,#13393,#13394,#13395,#13396,
#13397,#13398,#13399,#13400),.UNSPECIFIED.,.F.,.F.,(4,2,2,2,2,2,2,2,2,4),
(0.140389663816896,0.211667950083815,0.317493899242379,0.423319848400943,
0.529145797559505,0.634971746718067,0.740805721759974,0.846639696801881,
0.952473671843789,0.987029360618753),.UNSPECIFIED.);
#461=B_SPLINE_CURVE_WITH_KNOTS('',3,(#13401,#13402,#13403,#13404,#13405,
#13406,#13407,#13408,#13409,#13410,#13411,#13412,#13413,#13414,#13415,#13416,
#13417,#13418,#13419,#13420,#13421),.UNSPECIFIED.,.F.,.F.,(4,2,2,2,2,2,
2,3,2,4),(0.987029360618753,1.0583076468857,1.16413359604426,1.26995954520282,
1.37578549436138,1.48161144351995,1.58744541856186,1.69327939360377,1.79911336864567,
1.83366905742066),.UNSPECIFIED.);
#462=B_SPLINE_CURVE_WITH_KNOTS('',3,(#13424,#13425,#13426,#13427,#13428,
#13429,#13430,#13431,#13432,#13433,#13434,#13435,#13436,#13437,#13438,#13439,
#13440,#13441,#13442,#13443),.UNSPECIFIED.,.F.,.F.,(4,2,2,2,2,2,2,2,2,4),
(0.14038966381692,0.211667950083817,0.317493899242381,0.423319848400946,
0.529145797559508,0.634971746718069,0.740805721759977,0.846639696801884,
0.952473671843792,0.987029360618756),.UNSPECIFIED.);
#463=B_SPLINE_CURVE_WITH_KNOTS('',3,(#13444,#13445,#13446,#13447,#13448,
#13449,#13450,#13451,#13452,#13453,#13454,#13455,#13456,#13457,#13458,#13459,
#13460,#13461,#13462,#13463,#13464),.UNSPECIFIED.,.F.,.F.,(4,2,2,2,2,2,
2,3,2,4),(0.987029360618756,1.0583076468857,1.16413359604426,1.26995954520282,
1.37578549436139,1.48161144351995,1.58744541856186,1.69327939360377,1.79911336864568,
1.83366905742069),.UNSPECIFIED.);
#464=B_SPLINE_CURVE_WITH_KNOTS('',3,(#13467,#13468,#13469,#13470,#13471,
#13472,#13473,#13474,#13475,#13476,#13477,#13478,#13479,#13480,#13481,#13482,
#13483,#13484,#13485,#13486,#13487),.UNSPECIFIED.,.F.,.F.,(4,2,2,2,3,2,
2,2,2,4),(1.63431795680214,1.63484051213073,1.74655213492764,1.90358589296679,
2.06061965100595,2.19559646985844,2.33057328871092,2.44200600177386,2.5534387148368,
2.66004451397959),.UNSPECIFIED.);
#465=B_SPLINE_CURVE_WITH_KNOTS('',3,(#13488,#13489,#13490,#13491,#13492,
#13493,#13494,#13495,#13496,#13497,#13498,#13499,#13500,#13501,#13502,#13503,
#13504,#13505,#13506,#13507,#13508,#13509,#13510,#13511),.UNSPECIFIED.,
 .F.,.F.,(4,2,2,2,2,2,2,2,2,2,2,4),(2.66004451397959,2.66487142789973,2.77630414096267,
2.91128095981515,3.04625777866764,3.2032915367068,3.36032529474595,3.47203691754286,
3.52789272894132,3.58374854033977,3.63960435173823,3.69493760780809),
 .UNSPECIFIED.);
#466=B_SPLINE_CURVE_WITH_KNOTS('',3,(#13514,#13515,#13516,#13517,#13518,
#13519,#13520,#13521,#13522,#13523,#13524,#13525,#13526,#13527,#13528,#13529,
#13530,#13531,#13532,#13533,#13534),.UNSPECIFIED.,.F.,.F.,(4,2,2,3,2,2,
2,2,2,4),(1.48658026968317,1.57668032617585,1.70181043495793,1.82694054374001,
1.9422984039462,2.0576562641524,2.16466765320846,2.27167904226452,2.37869043132058,
2.39673280800115),.UNSPECIFIED.);
#467=B_SPLINE_CURVE_WITH_KNOTS('',3,(#13535,#13536,#13537,#13538,#13539,
#13540,#13541,#13542,#13543,#13544,#13545,#13546,#13547,#13548,#13549,#13550,
#13551,#13552,#13553,#13554),.UNSPECIFIED.,.F.,.F.,(4,2,2,2,2,2,2,2,2,4),
(2.39673280800115,2.48570182037664,2.60105968058283,2.71641754078903,2.84154764957111,
2.96667775835319,3.07591353624386,3.18514931413453,3.29438509202519,3.31352081342317),
 .UNSPECIFIED.);
#468=B_SPLINE_CURVE_WITH_KNOTS('',3,(#13557,#13558,#13559,#13560,#13561,
#13562,#13563,#13564,#13565,#13566,#13567,#13568,#13569,#13570,#13571,#13572,
#13573,#13574,#13575,#13576,#13577),.UNSPECIFIED.,.F.,.F.,(4,2,2,3,2,2,
2,2,2,4),(1.42506934481545,1.50220099251643,1.61276096598296,1.72332093944948,
1.83050112648501,1.93768131352053,2.04324956210919,2.14881781069785,2.25438605928651,
2.28497277338716),.UNSPECIFIED.);
#469=B_SPLINE_CURVE_WITH_KNOTS('',3,(#13578,#13579,#13580,#13581,#13582,
#13583,#13584,#13585,#13586,#13587,#13588,#13589,#13590,#13591,#13592,#13593,
#13594,#13595,#13596,#13597),.UNSPECIFIED.,.F.,.F.,(4,2,2,2,2,2,2,2,2,4),
(2.28497277338716,2.35995430787516,2.46713449491069,2.57431468194622,2.68487465541274,
2.79543462887926,2.90295645465092,3.01047828042259,3.11800010619425,3.14839028426493),
 .UNSPECIFIED.);
#470=B_SPLINE_CURVE_WITH_KNOTS('',3,(#13600,#13601,#13602,#13603,#13604,
#13605,#13606,#13607,#13608,#13609,#13610,#13611,#13612,#13613,#13614,#13615,
#13616,#13617,#13618,#13619),.UNSPECIFIED.,.F.,.F.,(4,2,2,2,2,2,2,2,2,4),
(0.140389663816901,0.211667950083817,0.31749389924238,0.423319848400942,
0.529145797559504,0.634971746718067,0.740805721759975,0.846639696801883,
0.952473671843791,0.987029360618755),.UNSPECIFIED.);
#471=B_SPLINE_CURVE_WITH_KNOTS('',3,(#13620,#13621,#13622,#13623,#13624,
#13625,#13626,#13627,#13628,#13629,#13630,#13631,#13632,#13633,#13634,#13635,
#13636,#13637,#13638,#13639,#13640),.UNSPECIFIED.,.F.,.F.,(4,2,2,2,2,2,
2,3,2,4),(0.987029360618755,1.0583076468857,1.16413359604426,1.26995954520283,
1.37578549436139,1.48161144351995,1.58744541856186,1.69327939360377,1.79911336864568,
1.83366905742067),.UNSPECIFIED.);
#472=B_SPLINE_CURVE_WITH_KNOTS('',3,(#13667,#13668,#13669,#13670,#13671,
#13672,#13673,#13674,#13675,#13676,#13677,#13678,#13679,#13680,#13681,#13682,
#13683,#13684),.UNSPECIFIED.,.F.,.F.,(4,2,2,2,2,2,2,2,4),(-2.42440986895005,
-2.27286833474305,-2.12132680053606,-1.96981710112429,-1.81830740171253,
-1.66679770230077,-1.51528800288901,-1.36374646868202,-1.21220493447502),
 .UNSPECIFIED.);
#473=B_SPLINE_CURVE_WITH_KNOTS('',3,(#13696,#13697,#13698,#13699,#13700,
#13701,#13702,#13703,#13704,#13705,#13706,#13707,#13708,#13709,#13710,#13711,
#13712,#13713),.UNSPECIFIED.,.F.,.F.,(4,2,2,2,2,2,2,2,4),(-2.42440986895003,
-2.27286833474304,-2.12132680053605,-1.96981710112428,-1.81830740171252,
-1.66679770230076,-1.515288002889,-1.36374646868201,-1.21220493447502),
 .UNSPECIFIED.);
#474=B_SPLINE_CURVE_WITH_KNOTS('',3,(#13863,#13864,#13865,#13866,#13867,
#13868,#13869,#13870,#13871,#13872,#13873,#13874,#13875,#13876,#13877,#13878,
#13879,#13880,#13881,#13882,#13883,#13884,#13885,#13886,#13887,#13888,#13889,
#13890),.UNSPECIFIED.,.F.,.F.,(4,2,2,2,2,2,2,2,2,2,2,2,2,4),(-1.08391055751389,
-1.04041495858034,-0.976127049627852,-0.875975346180159,-0.713802892781725,
-0.606446034139209,-0.5422685089836,-0.478121096415875,-0.370996668444261,
-0.213675448646841,-0.11261366027741,-0.0448303332672381,-0.0212473968071398,
0.),.UNSPECIFIED.);
#475=B_SPLINE_CURVE_WITH_KNOTS('',3,(#13926,#13927,#13928,#13929,#13930,
#13931,#13932,#13933,#13934,#13935,#13936,#13937,#13938,#13939,#13940,#13941,
#13942,#13943,#13944,#13945,#13946,#13947,#13948,#13949,#13950,#13951,#13952,
#13953),.UNSPECIFIED.,.F.,.F.,(4,2,2,2,2,2,2,2,2,2,2,2,2,4),(-1.08391055750046,
-1.04041495856732,-0.976127049615459,-0.875975346168904,-0.713802892772233,
-0.606446034130957,-0.542268508976211,-0.478121096409307,-0.370996668439296,
-0.213675448644088,-0.112613660276149,-0.0448303332669679,-0.0212473968071859,
0.),.UNSPECIFIED.);
#476=B_SPLINE_CURVE_WITH_KNOTS('',3,(#13989,#13990,#13991,#13992,#13993,
#13994,#13995,#13996,#13997,#13998,#13999,#14000,#14001,#14002,#14003,#14004,
#14005,#14006,#14007,#14008,#14009,#14010,#14011,#14012,#14013,#14014,#14015,
#14016),.UNSPECIFIED.,.F.,.F.,(4,2,2,2,2,2,2,2,2,2,2,2,2,4),(-1.0839105575165,
-1.04041495858262,-0.976127049629671,-0.8759753461813,-0.713802892781876,
-0.606446034138857,-0.542268508983049,-0.478121096415206,-0.370996668443923,
-0.21367544864674,-0.112613660277534,-0.0448303332674202,-0.021247396807171,
0.),.UNSPECIFIED.);
#477=CYLINDRICAL_SURFACE('',#6280,14.);
#478=CYLINDRICAL_SURFACE('',#6283,13.897506768291);
#479=CYLINDRICAL_SURFACE('',#6285,50.0401279512714);
#480=CYLINDRICAL_SURFACE('',#6301,109.542028553823);
#481=CYLINDRICAL_SURFACE('',#6302,109.542028553823);
#482=CYLINDRICAL_SURFACE('',#6303,37.);
#483=CYLINDRICAL_SURFACE('',#6304,50.0401279512714);
#484=CYLINDRICAL_SURFACE('',#6307,65.8399949356644);
#485=CYLINDRICAL_SURFACE('',#6308,65.8399949356645);
#486=CYLINDRICAL_SURFACE('',#6309,109.542028553823);
#487=CYLINDRICAL_SURFACE('',#6310,109.542028553823);
#488=CYLINDRICAL_SURFACE('',#6311,37.);
#489=CYLINDRICAL_SURFACE('',#6318,17.5);
#490=CYLINDRICAL_SURFACE('',#6322,17.5);
#491=CYLINDRICAL_SURFACE('',#6325,13.897506768291);
#492=CYLINDRICAL_SURFACE('',#6328,20.);
#493=CYLINDRICAL_SURFACE('',#6332,3.99999999999999);
#494=CYLINDRICAL_SURFACE('',#6333,15.9631510575949);
#495=CYLINDRICAL_SURFACE('',#6334,3.99999999999999);
#496=CYLINDRICAL_SURFACE('',#6335,3.99999999999999);
#497=CYLINDRICAL_SURFACE('',#6336,15.9631510575949);
#498=CYLINDRICAL_SURFACE('',#6337,3.99999999999999);
#499=CYLINDRICAL_SURFACE('',#6339,20.5);
#500=CYLINDRICAL_SURFACE('',#6357,1.02425693042952);
#501=CYLINDRICAL_SURFACE('',#6364,1.);
#502=CYLINDRICAL_SURFACE('',#6367,1.);
#503=CYLINDRICAL_SURFACE('',#6368,1.02425693042952);
#504=CYLINDRICAL_SURFACE('',#6375,1.02425693042952);
#505=CYLINDRICAL_SURFACE('',#6382,1.02425693042952);
#506=CYLINDRICAL_SURFACE('',#6389,1.);
#507=CYLINDRICAL_SURFACE('',#6392,1.);
#508=CYLINDRICAL_SURFACE('',#6393,1.);
#509=CYLINDRICAL_SURFACE('',#6396,1.);
#510=CYLINDRICAL_SURFACE('',#6397,1.);
#511=CYLINDRICAL_SURFACE('',#6400,1.);
#512=CYLINDRICAL_SURFACE('',#6405,17.5);
#513=CYLINDRICAL_SURFACE('',#6409,20.5);
#514=CYLINDRICAL_SURFACE('',#6428,1.02425693042952);
#515=CYLINDRICAL_SURFACE('',#6435,1.);
#516=CYLINDRICAL_SURFACE('',#6438,1.);
#517=CYLINDRICAL_SURFACE('',#6439,1.02425693042952);
#518=CYLINDRICAL_SURFACE('',#6446,1.02425693042952);
#519=CYLINDRICAL_SURFACE('',#6453,1.02425693042952);
#520=CYLINDRICAL_SURFACE('',#6460,1.);
#521=CYLINDRICAL_SURFACE('',#6463,1.);
#522=CYLINDRICAL_SURFACE('',#6464,1.);
#523=CYLINDRICAL_SURFACE('',#6467,1.);
#524=CYLINDRICAL_SURFACE('',#6468,1.);
#525=CYLINDRICAL_SURFACE('',#6471,1.);
#526=CYLINDRICAL_SURFACE('',#6476,17.5);
#527=CYLINDRICAL_SURFACE('',#6483,10.9999999999984);
#528=CYLINDRICAL_SURFACE('',#6486,13.0000000000012);
#529=CYLINDRICAL_SURFACE('',#6493,10.9999999999984);
#530=CYLINDRICAL_SURFACE('',#6496,13.0000000000012);
#531=CYLINDRICAL_SURFACE('',#6503,10.9999999999984);
#532=CYLINDRICAL_SURFACE('',#6506,13.0000000000012);
#533=CYLINDRICAL_SURFACE('',#6509,15.);
#534=CYLINDRICAL_SURFACE('',#6512,15.);
#535=CYLINDRICAL_SURFACE('',#6515,15.);
#536=CYLINDRICAL_SURFACE('',#6520,15.);
#537=CYLINDRICAL_SURFACE('',#6523,15.);
#538=CYLINDRICAL_SURFACE('',#6526,15.);
#539=CYLINDRICAL_SURFACE('',#6531,15.);
#540=CYLINDRICAL_SURFACE('',#6534,15.);
#541=CYLINDRICAL_SURFACE('',#6537,15.);
#542=CYLINDRICAL_SURFACE('',#6542,28.1634258170599);
#543=CYLINDRICAL_SURFACE('',#6549,23.1634258170599);
#544=CYLINDRICAL_SURFACE('',#6552,15.);
#545=CYLINDRICAL_SURFACE('',#6556,17.);
#546=CYLINDRICAL_SURFACE('',#6559,13.);
#547=CYLINDRICAL_SURFACE('',#6561,15.);
#548=CYLINDRICAL_SURFACE('',#6563,15.);
#549=CYLINDRICAL_SURFACE('',#6567,17.);
#550=CYLINDRICAL_SURFACE('',#6572,17.);
#551=CYLINDRICAL_SURFACE('',#6575,13.);
#552=CYLINDRICAL_SURFACE('',#6576,13.);
#553=CYLINDRICAL_SURFACE('',#6581,20.);
#554=CYLINDRICAL_SURFACE('',#6610,3.99999999999999);
#555=CYLINDRICAL_SURFACE('',#6617,0.899999999999993);
#556=CYLINDRICAL_SURFACE('',#6623,3.49999999999999);
#557=CYLINDRICAL_SURFACE('',#6625,4.00000000000001);
#558=CYLINDRICAL_SURFACE('',#6632,0.899999999999993);
#559=CYLINDRICAL_SURFACE('',#6638,3.50000000000001);
#560=CYLINDRICAL_SURFACE('',#6640,4.);
#561=CYLINDRICAL_SURFACE('',#6647,0.899999999999989);
#562=CYLINDRICAL_SURFACE('',#6653,3.49999999999993);
#563=CYLINDRICAL_SURFACE('',#6655,4.00000000000013);
#564=CYLINDRICAL_SURFACE('',#6662,0.899999999999984);
#565=CYLINDRICAL_SURFACE('',#6668,3.50000000000012);
#566=CYLINDRICAL_SURFACE('',#6670,15.);
#567=CYLINDRICAL_SURFACE('',#6673,15.);
#568=CYLINDRICAL_SURFACE('',#6676,15.);
#569=CYLINDRICAL_SURFACE('',#6679,15.);
#570=CYLINDRICAL_SURFACE('',#6680,15.);
#571=CYLINDRICAL_SURFACE('',#6681,15.);
#572=CYLINDRICAL_SURFACE('',#6682,15.);
#573=CYLINDRICAL_SURFACE('',#6683,15.);
#574=CYLINDRICAL_SURFACE('',#6686,15.);
#575=CYLINDRICAL_SURFACE('',#6687,15.);
#576=CYLINDRICAL_SURFACE('',#6688,15.);
#577=CYLINDRICAL_SURFACE('',#6689,15.);
#578=CYLINDRICAL_SURFACE('',#6690,15.);
#579=CYLINDRICAL_SURFACE('',#6691,15.);
#580=CYLINDRICAL_SURFACE('',#6692,15.);
#581=CYLINDRICAL_SURFACE('',#6693,15.);
#582=CYLINDRICAL_SURFACE('',#6694,15.);
#583=CYLINDRICAL_SURFACE('',#6697,15.);
#584=CYLINDRICAL_SURFACE('',#6707,17.);
#585=CYLINDRICAL_SURFACE('',#6717,4.00000000000012);
#586=CYLINDRICAL_SURFACE('',#6721,4.00000000000001);
#587=CYLINDRICAL_SURFACE('',#6725,4.00000000000001);
#588=CYLINDRICAL_SURFACE('',#6729,4.);
#589=CYLINDRICAL_SURFACE('',#6733,3.50000000000012);
#590=CYLINDRICAL_SURFACE('',#6737,3.5);
#591=CYLINDRICAL_SURFACE('',#6741,3.49999999999992);
#592=CYLINDRICAL_SURFACE('',#6742,12.9999999999984);
#593=CYLINDRICAL_SURFACE('',#6748,3.49999999999998);
#594=CYLINDRICAL_SURFACE('',#6749,2.80000000000012);
#595=CYLINDRICAL_SURFACE('',#6750,2.79999999999998);
#596=CYLINDRICAL_SURFACE('',#6751,2.79999999999991);
#597=CYLINDRICAL_SURFACE('',#6752,2.79999999999999);
#598=CYLINDRICAL_SURFACE('',#6756,4.00000000000012);
#599=CYLINDRICAL_SURFACE('',#6760,4.00000000000012);
#600=CYLINDRICAL_SURFACE('',#6764,4.00000000000001);
#601=CYLINDRICAL_SURFACE('',#6768,4.00000000000001);
#602=CYLINDRICAL_SURFACE('',#6772,4.00000000000001);
#603=CYLINDRICAL_SURFACE('',#6776,4.00000000000001);
#604=CYLINDRICAL_SURFACE('',#6780,4.);
#605=CYLINDRICAL_SURFACE('',#6784,4.);
#606=CYLINDRICAL_SURFACE('',#6785,2.80000000000012);
#607=CYLINDRICAL_SURFACE('',#6787,2.80000000000012);
#608=CYLINDRICAL_SURFACE('',#6789,2.79999999999998);
#609=CYLINDRICAL_SURFACE('',#6791,2.79999999999998);
#610=CYLINDRICAL_SURFACE('',#6793,2.79999999999991);
#611=CYLINDRICAL_SURFACE('',#6795,2.79999999999991);
#612=CYLINDRICAL_SURFACE('',#6797,2.79999999999999);
#613=CYLINDRICAL_SURFACE('',#6799,2.79999999999999);
#614=CYLINDRICAL_SURFACE('',#6803,3.50000000000012);
#615=CYLINDRICAL_SURFACE('',#6806,3.50000000000012);
#616=CYLINDRICAL_SURFACE('',#6809,3.5);
#617=CYLINDRICAL_SURFACE('',#6812,3.5);
#618=CYLINDRICAL_SURFACE('',#6815,3.49999999999992);
#619=CYLINDRICAL_SURFACE('',#6818,3.49999999999992);
#620=CYLINDRICAL_SURFACE('',#6821,3.49999999999998);
#621=CYLINDRICAL_SURFACE('',#6824,3.49999999999998);
#622=CYLINDRICAL_SURFACE('',#6829,14.5);
#623=CYLINDRICAL_SURFACE('',#6834,14.5);
#624=CYLINDRICAL_SURFACE('',#6839,14.5);
#625=CYLINDRICAL_SURFACE('',#6897,14.);
#626=CYLINDRICAL_SURFACE('',#6901,12.);
#627=FACE_BOUND('',#1086,.T.);
#628=FACE_BOUND('',#1087,.T.);
#629=FACE_BOUND('',#1088,.T.);
#630=FACE_BOUND('',#1090,.T.);
#631=FACE_BOUND('',#1091,.T.);
#632=FACE_BOUND('',#1092,.T.);
#633=FACE_BOUND('',#1093,.T.);
#634=FACE_BOUND('',#1094,.T.);
#635=FACE_BOUND('',#1095,.T.);
#636=FACE_BOUND('',#1096,.T.);
#637=FACE_BOUND('',#1097,.T.);
#638=FACE_BOUND('',#1099,.T.);
#639=FACE_BOUND('',#1100,.T.);
#640=FACE_BOUND('',#1104,.T.);
#641=FACE_BOUND('',#1105,.T.);
#642=FACE_BOUND('',#1106,.T.);
#643=FACE_BOUND('',#1138,.T.);
#644=FACE_BOUND('',#1141,.T.);
#645=FACE_BOUND('',#1144,.T.);
#646=FACE_BOUND('',#1156,.T.);
#647=FACE_BOUND('',#1157,.T.);
#648=FACE_BOUND('',#1158,.T.);
#649=FACE_BOUND('',#1159,.T.);
#650=FACE_BOUND('',#1160,.T.);
#651=FACE_BOUND('',#1161,.T.);
#652=FACE_BOUND('',#1162,.T.);
#653=FACE_BOUND('',#1165,.T.);
#654=FACE_BOUND('',#1203,.T.);
#655=FACE_BOUND('',#1204,.T.);
#656=FACE_BOUND('',#1205,.T.);
#657=FACE_BOUND('',#1206,.T.);
#658=FACE_BOUND('',#1207,.T.);
#659=FACE_BOUND('',#1208,.T.);
#660=FACE_BOUND('',#1209,.T.);
#661=FACE_BOUND('',#1211,.T.);
#662=FACE_BOUND('',#1213,.T.);
#663=FACE_BOUND('',#1271,.T.);
#664=FACE_BOUND('',#1276,.T.);
#665=FACE_BOUND('',#1281,.T.);
#666=FACE_BOUND('',#1283,.T.);
#667=FACE_BOUND('',#1284,.T.);
#668=FACE_BOUND('',#1286,.T.);
#669=FACE_BOUND('',#1288,.T.);
#670=FACE_BOUND('',#1293,.T.);
#671=FACE_BOUND('',#1300,.T.);
#672=FACE_BOUND('',#1303,.T.);
#673=FACE_BOUND('',#1311,.T.);
#674=FACE_BOUND('',#1312,.T.);
#675=FACE_BOUND('',#1342,.T.);
#676=FACE_BOUND('',#1344,.T.);
#677=FACE_BOUND('',#1348,.T.);
#678=FACE_BOUND('',#1352,.T.);
#679=FACE_BOUND('',#1354,.T.);
#680=FACE_BOUND('',#1358,.T.);
#681=FACE_BOUND('',#1362,.T.);
#682=FACE_BOUND('',#1364,.T.);
#683=FACE_BOUND('',#1368,.T.);
#684=FACE_BOUND('',#1372,.T.);
#685=FACE_BOUND('',#1374,.T.);
#686=FACE_BOUND('',#1378,.T.);
#687=FACE_BOUND('',#1399,.T.);
#688=FACE_BOUND('',#1401,.T.);
#689=FACE_BOUND('',#1404,.T.);
#690=FACE_BOUND('',#1407,.T.);
#691=FACE_BOUND('',#1410,.T.);
#692=FACE_BOUND('',#1413,.T.);
#693=FACE_BOUND('',#1416,.T.);
#694=FACE_BOUND('',#1419,.T.);
#695=FACE_BOUND('',#1422,.T.);
#696=FACE_BOUND('',#1425,.T.);
#697=FACE_BOUND('',#1428,.T.);
#698=FACE_BOUND('',#1429,.T.);
#699=FACE_BOUND('',#1430,.T.);
#700=FACE_BOUND('',#1431,.T.);
#701=FACE_BOUND('',#1432,.T.);
#702=FACE_BOUND('',#1433,.T.);
#703=FACE_BOUND('',#1434,.T.);
#704=FACE_BOUND('',#1435,.T.);
#705=FACE_BOUND('',#1436,.T.);
#706=FACE_BOUND('',#1437,.T.);
#707=FACE_BOUND('',#1438,.T.);
#708=FACE_BOUND('',#1439,.T.);
#709=FACE_BOUND('',#1442,.T.);
#710=FACE_BOUND('',#1449,.T.);
#711=FACE_BOUND('',#1452,.T.);
#712=FACE_BOUND('',#1455,.T.);
#713=FACE_BOUND('',#1458,.T.);
#714=FACE_BOUND('',#1461,.T.);
#715=FACE_BOUND('',#1464,.T.);
#716=FACE_BOUND('',#1467,.T.);
#717=FACE_BOUND('',#1470,.T.);
#718=FACE_BOUND('',#1481,.T.);
#719=FACE_BOUND('',#1484,.T.);
#720=FACE_BOUND('',#1487,.T.);
#721=FACE_BOUND('',#1490,.T.);
#722=FACE_BOUND('',#1493,.T.);
#723=FACE_BOUND('',#1496,.T.);
#724=FACE_BOUND('',#1499,.T.);
#725=FACE_BOUND('',#1502,.T.);
#726=FACE_BOUND('',#1510,.T.);
#727=FACE_BOUND('',#1517,.T.);
#728=FACE_BOUND('',#1524,.T.);
#729=FACE_BOUND('',#1536,.T.);
#730=FACE_BOUND('',#1538,.T.);
#731=FACE_BOUND('',#1541,.T.);
#732=FACE_OUTER_BOUND('',#1085,.T.);
#733=FACE_OUTER_BOUND('',#1089,.T.);
#734=FACE_OUTER_BOUND('',#1098,.T.);
#735=FACE_OUTER_BOUND('',#1101,.T.);
#736=FACE_OUTER_BOUND('',#1102,.T.);
#737=FACE_OUTER_BOUND('',#1103,.T.);
#738=FACE_OUTER_BOUND('',#1107,.T.);
#739=FACE_OUTER_BOUND('',#1108,.T.);
#740=FACE_OUTER_BOUND('',#1109,.T.);
#741=FACE_OUTER_BOUND('',#1110,.T.);
#742=FACE_OUTER_BOUND('',#1111,.T.);
#743=FACE_OUTER_BOUND('',#1112,.T.);
#744=FACE_OUTER_BOUND('',#1113,.T.);
#745=FACE_OUTER_BOUND('',#1114,.T.);
#746=FACE_OUTER_BOUND('',#1115,.T.);
#747=FACE_OUTER_BOUND('',#1116,.T.);
#748=FACE_OUTER_BOUND('',#1117,.T.);
#749=FACE_OUTER_BOUND('',#1118,.T.);
#750=FACE_OUTER_BOUND('',#1119,.T.);
#751=FACE_OUTER_BOUND('',#1120,.T.);
#752=FACE_OUTER_BOUND('',#1121,.T.);
#753=FACE_OUTER_BOUND('',#1122,.T.);
#754=FACE_OUTER_BOUND('',#1123,.T.);
#755=FACE_OUTER_BOUND('',#1124,.T.);
#756=FACE_OUTER_BOUND('',#1125,.T.);
#757=FACE_OUTER_BOUND('',#1126,.T.);
#758=FACE_OUTER_BOUND('',#1127,.T.);
#759=FACE_OUTER_BOUND('',#1128,.T.);
#760=FACE_OUTER_BOUND('',#1129,.T.);
#761=FACE_OUTER_BOUND('',#1130,.T.);
#762=FACE_OUTER_BOUND('',#1131,.T.);
#763=FACE_OUTER_BOUND('',#1132,.T.);
#764=FACE_OUTER_BOUND('',#1133,.T.);
#765=FACE_OUTER_BOUND('',#1134,.T.);
#766=FACE_OUTER_BOUND('',#1135,.T.);
#767=FACE_OUTER_BOUND('',#1136,.T.);
#768=FACE_OUTER_BOUND('',#1137,.T.);
#769=FACE_OUTER_BOUND('',#1139,.T.);
#770=FACE_OUTER_BOUND('',#1140,.T.);
#771=FACE_OUTER_BOUND('',#1142,.T.);
#772=FACE_OUTER_BOUND('',#1143,.T.);
#773=FACE_OUTER_BOUND('',#1145,.T.);
#774=FACE_OUTER_BOUND('',#1146,.T.);
#775=FACE_OUTER_BOUND('',#1147,.T.);
#776=FACE_OUTER_BOUND('',#1148,.T.);
#777=FACE_OUTER_BOUND('',#1149,.T.);
#778=FACE_OUTER_BOUND('',#1150,.T.);
#779=FACE_OUTER_BOUND('',#1151,.T.);
#780=FACE_OUTER_BOUND('',#1152,.T.);
#781=FACE_OUTER_BOUND('',#1153,.T.);
#782=FACE_OUTER_BOUND('',#1154,.T.);
#783=FACE_OUTER_BOUND('',#1155,.T.);
#784=FACE_OUTER_BOUND('',#1163,.T.);
#785=FACE_OUTER_BOUND('',#1164,.T.);
#786=FACE_OUTER_BOUND('',#1166,.T.);
#787=FACE_OUTER_BOUND('',#1167,.T.);
#788=FACE_OUTER_BOUND('',#1168,.T.);
#789=FACE_OUTER_BOUND('',#1169,.T.);
#790=FACE_OUTER_BOUND('',#1170,.T.);
#791=FACE_OUTER_BOUND('',#1171,.T.);
#792=FACE_OUTER_BOUND('',#1172,.T.);
#793=FACE_OUTER_BOUND('',#1173,.T.);
#794=FACE_OUTER_BOUND('',#1174,.T.);
#795=FACE_OUTER_BOUND('',#1175,.T.);
#796=FACE_OUTER_BOUND('',#1176,.T.);
#797=FACE_OUTER_BOUND('',#1177,.T.);
#798=FACE_OUTER_BOUND('',#1178,.T.);
#799=FACE_OUTER_BOUND('',#1179,.T.);
#800=FACE_OUTER_BOUND('',#1180,.T.);
#801=FACE_OUTER_BOUND('',#1181,.T.);
#802=FACE_OUTER_BOUND('',#1182,.T.);
#803=FACE_OUTER_BOUND('',#1183,.T.);
#804=FACE_OUTER_BOUND('',#1184,.T.);
#805=FACE_OUTER_BOUND('',#1185,.T.);
#806=FACE_OUTER_BOUND('',#1186,.T.);
#807=FACE_OUTER_BOUND('',#1187,.T.);
#808=FACE_OUTER_BOUND('',#1188,.T.);
#809=FACE_OUTER_BOUND('',#1189,.T.);
#810=FACE_OUTER_BOUND('',#1190,.T.);
#811=FACE_OUTER_BOUND('',#1191,.T.);
#812=FACE_OUTER_BOUND('',#1192,.T.);
#813=FACE_OUTER_BOUND('',#1193,.T.);
#814=FACE_OUTER_BOUND('',#1194,.T.);
#815=FACE_OUTER_BOUND('',#1195,.T.);
#816=FACE_OUTER_BOUND('',#1196,.T.);
#817=FACE_OUTER_BOUND('',#1197,.T.);
#818=FACE_OUTER_BOUND('',#1198,.T.);
#819=FACE_OUTER_BOUND('',#1199,.T.);
#820=FACE_OUTER_BOUND('',#1200,.T.);
#821=FACE_OUTER_BOUND('',#1201,.T.);
#822=FACE_OUTER_BOUND('',#1202,.T.);
#823=FACE_OUTER_BOUND('',#1210,.T.);
#824=FACE_OUTER_BOUND('',#1212,.T.);
#825=FACE_OUTER_BOUND('',#1214,.T.);
#826=FACE_OUTER_BOUND('',#1215,.T.);
#827=FACE_OUTER_BOUND('',#1216,.T.);
#828=FACE_OUTER_BOUND('',#1217,.T.);
#829=FACE_OUTER_BOUND('',#1218,.T.);
#830=FACE_OUTER_BOUND('',#1219,.T.);
#831=FACE_OUTER_BOUND('',#1220,.T.);
#832=FACE_OUTER_BOUND('',#1221,.T.);
#833=FACE_OUTER_BOUND('',#1222,.T.);
#834=FACE_OUTER_BOUND('',#1223,.T.);
#835=FACE_OUTER_BOUND('',#1224,.T.);
#836=FACE_OUTER_BOUND('',#1225,.T.);
#837=FACE_OUTER_BOUND('',#1226,.T.);
#838=FACE_OUTER_BOUND('',#1227,.T.);
#839=FACE_OUTER_BOUND('',#1228,.T.);
#840=FACE_OUTER_BOUND('',#1229,.T.);
#841=FACE_OUTER_BOUND('',#1230,.T.);
#842=FACE_OUTER_BOUND('',#1231,.T.);
#843=FACE_OUTER_BOUND('',#1232,.T.);
#844=FACE_OUTER_BOUND('',#1233,.T.);
#845=FACE_OUTER_BOUND('',#1234,.T.);
#846=FACE_OUTER_BOUND('',#1235,.T.);
#847=FACE_OUTER_BOUND('',#1236,.T.);
#848=FACE_OUTER_BOUND('',#1237,.T.);
#849=FACE_OUTER_BOUND('',#1238,.T.);
#850=FACE_OUTER_BOUND('',#1239,.T.);
#851=FACE_OUTER_BOUND('',#1240,.T.);
#852=FACE_OUTER_BOUND('',#1241,.T.);
#853=FACE_OUTER_BOUND('',#1242,.T.);
#854=FACE_OUTER_BOUND('',#1243,.T.);
#855=FACE_OUTER_BOUND('',#1244,.T.);
#856=FACE_OUTER_BOUND('',#1245,.T.);
#857=FACE_OUTER_BOUND('',#1246,.T.);
#858=FACE_OUTER_BOUND('',#1247,.T.);
#859=FACE_OUTER_BOUND('',#1248,.T.);
#860=FACE_OUTER_BOUND('',#1249,.T.);
#861=FACE_OUTER_BOUND('',#1250,.T.);
#862=FACE_OUTER_BOUND('',#1251,.T.);
#863=FACE_OUTER_BOUND('',#1252,.T.);
#864=FACE_OUTER_BOUND('',#1253,.T.);
#865=FACE_OUTER_BOUND('',#1254,.T.);
#866=FACE_OUTER_BOUND('',#1255,.T.);
#867=FACE_OUTER_BOUND('',#1256,.T.);
#868=FACE_OUTER_BOUND('',#1257,.T.);
#869=FACE_OUTER_BOUND('',#1258,.T.);
#870=FACE_OUTER_BOUND('',#1259,.T.);
#871=FACE_OUTER_BOUND('',#1260,.T.);
#872=FACE_OUTER_BOUND('',#1261,.T.);
#873=FACE_OUTER_BOUND('',#1262,.T.);
#874=FACE_OUTER_BOUND('',#1263,.T.);
#875=FACE_OUTER_BOUND('',#1264,.T.);
#876=FACE_OUTER_BOUND('',#1265,.T.);
#877=FACE_OUTER_BOUND('',#1266,.T.);
#878=FACE_OUTER_BOUND('',#1267,.T.);
#879=FACE_OUTER_BOUND('',#1268,.T.);
#880=FACE_OUTER_BOUND('',#1269,.T.);
#881=FACE_OUTER_BOUND('',#1270,.T.);
#882=FACE_OUTER_BOUND('',#1272,.T.);
#883=FACE_OUTER_BOUND('',#1273,.T.);
#884=FACE_OUTER_BOUND('',#1274,.T.);
#885=FACE_OUTER_BOUND('',#1275,.T.);
#886=FACE_OUTER_BOUND('',#1277,.T.);
#887=FACE_OUTER_BOUND('',#1278,.T.);
#888=FACE_OUTER_BOUND('',#1279,.T.);
#889=FACE_OUTER_BOUND('',#1280,.T.);
#890=FACE_OUTER_BOUND('',#1282,.T.);
#891=FACE_OUTER_BOUND('',#1285,.T.);
#892=FACE_OUTER_BOUND('',#1287,.T.);
#893=FACE_OUTER_BOUND('',#1289,.T.);
#894=FACE_OUTER_BOUND('',#1290,.T.);
#895=FACE_OUTER_BOUND('',#1291,.T.);
#896=FACE_OUTER_BOUND('',#1292,.T.);
#897=FACE_OUTER_BOUND('',#1294,.T.);
#898=FACE_OUTER_BOUND('',#1295,.T.);
#899=FACE_OUTER_BOUND('',#1296,.T.);
#900=FACE_OUTER_BOUND('',#1297,.T.);
#901=FACE_OUTER_BOUND('',#1298,.T.);
#902=FACE_OUTER_BOUND('',#1299,.T.);
#903=FACE_OUTER_BOUND('',#1301,.T.);
#904=FACE_OUTER_BOUND('',#1302,.T.);
#905=FACE_OUTER_BOUND('',#1304,.T.);
#906=FACE_OUTER_BOUND('',#1305,.T.);
#907=FACE_OUTER_BOUND('',#1306,.T.);
#908=FACE_OUTER_BOUND('',#1307,.T.);
#909=FACE_OUTER_BOUND('',#1308,.T.);
#910=FACE_OUTER_BOUND('',#1309,.T.);
#911=FACE_OUTER_BOUND('',#1310,.T.);
#912=FACE_OUTER_BOUND('',#1313,.T.);
#913=FACE_OUTER_BOUND('',#1314,.T.);
#914=FACE_OUTER_BOUND('',#1315,.T.);
#915=FACE_OUTER_BOUND('',#1316,.T.);
#916=FACE_OUTER_BOUND('',#1317,.T.);
#917=FACE_OUTER_BOUND('',#1318,.T.);
#918=FACE_OUTER_BOUND('',#1319,.T.);
#919=FACE_OUTER_BOUND('',#1320,.T.);
#920=FACE_OUTER_BOUND('',#1321,.T.);
#921=FACE_OUTER_BOUND('',#1322,.T.);
#922=FACE_OUTER_BOUND('',#1323,.T.);
#923=FACE_OUTER_BOUND('',#1324,.T.);
#924=FACE_OUTER_BOUND('',#1325,.T.);
#925=FACE_OUTER_BOUND('',#1326,.T.);
#926=FACE_OUTER_BOUND('',#1327,.T.);
#927=FACE_OUTER_BOUND('',#1328,.T.);
#928=FACE_OUTER_BOUND('',#1329,.T.);
#929=FACE_OUTER_BOUND('',#1330,.T.);
#930=FACE_OUTER_BOUND('',#1331,.T.);
#931=FACE_OUTER_BOUND('',#1332,.T.);
#932=FACE_OUTER_BOUND('',#1333,.T.);
#933=FACE_OUTER_BOUND('',#1334,.T.);
#934=FACE_OUTER_BOUND('',#1335,.T.);
#935=FACE_OUTER_BOUND('',#1336,.T.);
#936=FACE_OUTER_BOUND('',#1337,.T.);
#937=FACE_OUTER_BOUND('',#1338,.T.);
#938=FACE_OUTER_BOUND('',#1339,.T.);
#939=FACE_OUTER_BOUND('',#1340,.T.);
#940=FACE_OUTER_BOUND('',#1341,.T.);
#941=FACE_OUTER_BOUND('',#1343,.T.);
#942=FACE_OUTER_BOUND('',#1345,.T.);
#943=FACE_OUTER_BOUND('',#1346,.T.);
#944=FACE_OUTER_BOUND('',#1347,.T.);
#945=FACE_OUTER_BOUND('',#1349,.T.);
#946=FACE_OUTER_BOUND('',#1350,.T.);
#947=FACE_OUTER_BOUND('',#1351,.T.);
#948=FACE_OUTER_BOUND('',#1353,.T.);
#949=FACE_OUTER_BOUND('',#1355,.T.);
#950=FACE_OUTER_BOUND('',#1356,.T.);
#951=FACE_OUTER_BOUND('',#1357,.T.);
#952=FACE_OUTER_BOUND('',#1359,.T.);
#953=FACE_OUTER_BOUND('',#1360,.T.);
#954=FACE_OUTER_BOUND('',#1361,.T.);
#955=FACE_OUTER_BOUND('',#1363,.T.);
#956=FACE_OUTER_BOUND('',#1365,.T.);
#957=FACE_OUTER_BOUND('',#1366,.T.);
#958=FACE_OUTER_BOUND('',#1367,.T.);
#959=FACE_OUTER_BOUND('',#1369,.T.);
#960=FACE_OUTER_BOUND('',#1370,.T.);
#961=FACE_OUTER_BOUND('',#1371,.T.);
#962=FACE_OUTER_BOUND('',#1373,.T.);
#963=FACE_OUTER_BOUND('',#1375,.T.);
#964=FACE_OUTER_BOUND('',#1376,.T.);
#965=FACE_OUTER_BOUND('',#1377,.T.);
#966=FACE_OUTER_BOUND('',#1379,.T.);
#967=FACE_OUTER_BOUND('',#1380,.T.);
#968=FACE_OUTER_BOUND('',#1381,.T.);
#969=FACE_OUTER_BOUND('',#1382,.T.);
#970=FACE_OUTER_BOUND('',#1383,.T.);
#971=FACE_OUTER_BOUND('',#1384,.T.);
#972=FACE_OUTER_BOUND('',#1385,.T.);
#973=FACE_OUTER_BOUND('',#1386,.T.);
#974=FACE_OUTER_BOUND('',#1387,.T.);
#975=FACE_OUTER_BOUND('',#1388,.T.);
#976=FACE_OUTER_BOUND('',#1389,.T.);
#977=FACE_OUTER_BOUND('',#1390,.T.);
#978=FACE_OUTER_BOUND('',#1391,.T.);
#979=FACE_OUTER_BOUND('',#1392,.T.);
#980=FACE_OUTER_BOUND('',#1393,.T.);
#981=FACE_OUTER_BOUND('',#1394,.T.);
#982=FACE_OUTER_BOUND('',#1395,.T.);
#983=FACE_OUTER_BOUND('',#1396,.T.);
#984=FACE_OUTER_BOUND('',#1397,.T.);
#985=FACE_OUTER_BOUND('',#1398,.T.);
#986=FACE_OUTER_BOUND('',#1400,.T.);
#987=FACE_OUTER_BOUND('',#1402,.T.);
#988=FACE_OUTER_BOUND('',#1403,.T.);
#989=FACE_OUTER_BOUND('',#1405,.T.);
#990=FACE_OUTER_BOUND('',#1406,.T.);
#991=FACE_OUTER_BOUND('',#1408,.T.);
#992=FACE_OUTER_BOUND('',#1409,.T.);
#993=FACE_OUTER_BOUND('',#1411,.T.);
#994=FACE_OUTER_BOUND('',#1412,.T.);
#995=FACE_OUTER_BOUND('',#1414,.T.);
#996=FACE_OUTER_BOUND('',#1415,.T.);
#997=FACE_OUTER_BOUND('',#1417,.T.);
#998=FACE_OUTER_BOUND('',#1418,.T.);
#999=FACE_OUTER_BOUND('',#1420,.T.);
#1000=FACE_OUTER_BOUND('',#1421,.T.);
#1001=FACE_OUTER_BOUND('',#1423,.T.);
#1002=FACE_OUTER_BOUND('',#1424,.T.);
#1003=FACE_OUTER_BOUND('',#1426,.T.);
#1004=FACE_OUTER_BOUND('',#1427,.T.);
#1005=FACE_OUTER_BOUND('',#1440,.T.);
#1006=FACE_OUTER_BOUND('',#1441,.T.);
#1007=FACE_OUTER_BOUND('',#1443,.T.);
#1008=FACE_OUTER_BOUND('',#1444,.T.);
#1009=FACE_OUTER_BOUND('',#1445,.T.);
#1010=FACE_OUTER_BOUND('',#1446,.T.);
#1011=FACE_OUTER_BOUND('',#1447,.T.);
#1012=FACE_OUTER_BOUND('',#1448,.T.);
#1013=FACE_OUTER_BOUND('',#1450,.T.);
#1014=FACE_OUTER_BOUND('',#1451,.T.);
#1015=FACE_OUTER_BOUND('',#1453,.T.);
#1016=FACE_OUTER_BOUND('',#1454,.T.);
#1017=FACE_OUTER_BOUND('',#1456,.T.);
#1018=FACE_OUTER_BOUND('',#1457,.T.);
#1019=FACE_OUTER_BOUND('',#1459,.T.);
#1020=FACE_OUTER_BOUND('',#1460,.T.);
#1021=FACE_OUTER_BOUND('',#1462,.T.);
#1022=FACE_OUTER_BOUND('',#1463,.T.);
#1023=FACE_OUTER_BOUND('',#1465,.T.);
#1024=FACE_OUTER_BOUND('',#1466,.T.);
#1025=FACE_OUTER_BOUND('',#1468,.T.);
#1026=FACE_OUTER_BOUND('',#1469,.T.);
#1027=FACE_OUTER_BOUND('',#1471,.T.);
#1028=FACE_OUTER_BOUND('',#1472,.T.);
#1029=FACE_OUTER_BOUND('',#1473,.T.);
#1030=FACE_OUTER_BOUND('',#1474,.T.);
#1031=FACE_OUTER_BOUND('',#1475,.T.);
#1032=FACE_OUTER_BOUND('',#1476,.T.);
#1033=FACE_OUTER_BOUND('',#1477,.T.);
#1034=FACE_OUTER_BOUND('',#1478,.T.);
#1035=FACE_OUTER_BOUND('',#1479,.T.);
#1036=FACE_OUTER_BOUND('',#1480,.T.);
#1037=FACE_OUTER_BOUND('',#1482,.T.);
#1038=FACE_OUTER_BOUND('',#1483,.T.);
#1039=FACE_OUTER_BOUND('',#1485,.T.);
#1040=FACE_OUTER_BOUND('',#1486,.T.);
#1041=FACE_OUTER_BOUND('',#1488,.T.);
#1042=FACE_OUTER_BOUND('',#1489,.T.);
#1043=FACE_OUTER_BOUND('',#1491,.T.);
#1044=FACE_OUTER_BOUND('',#1492,.T.);
#1045=FACE_OUTER_BOUND('',#1494,.T.);
#1046=FACE_OUTER_BOUND('',#1495,.T.);
#1047=FACE_OUTER_BOUND('',#1497,.T.);
#1048=FACE_OUTER_BOUND('',#1498,.T.);
#1049=FACE_OUTER_BOUND('',#1500,.T.);
#1050=FACE_OUTER_BOUND('',#1501,.T.);
#1051=FACE_OUTER_BOUND('',#1503,.T.);
#1052=FACE_OUTER_BOUND('',#1504,.T.);
#1053=FACE_OUTER_BOUND('',#1505,.T.);
#1054=FACE_OUTER_BOUND('',#1506,.T.);
#1055=FACE_OUTER_BOUND('',#1507,.T.);
#1056=FACE_OUTER_BOUND('',#1508,.T.);
#1057=FACE_OUTER_BOUND('',#1509,.T.);
#1058=FACE_OUTER_BOUND('',#1511,.T.);
#1059=FACE_OUTER_BOUND('',#1512,.T.);
#1060=FACE_OUTER_BOUND('',#1513,.T.);
#1061=FACE_OUTER_BOUND('',#1514,.T.);
#1062=FACE_OUTER_BOUND('',#1515,.T.);
#1063=FACE_OUTER_BOUND('',#1516,.T.);
#1064=FACE_OUTER_BOUND('',#1518,.T.);
#1065=FACE_OUTER_BOUND('',#1519,.T.);
#1066=FACE_OUTER_BOUND('',#1520,.T.);
#1067=FACE_OUTER_BOUND('',#1521,.T.);
#1068=FACE_OUTER_BOUND('',#1522,.T.);
#1069=FACE_OUTER_BOUND('',#1523,.T.);
#1070=FACE_OUTER_BOUND('',#1525,.T.);
#1071=FACE_OUTER_BOUND('',#1526,.T.);
#1072=FACE_OUTER_BOUND('',#1527,.T.);
#1073=FACE_OUTER_BOUND('',#1528,.T.);
#1074=FACE_OUTER_BOUND('',#1529,.T.);
#1075=FACE_OUTER_BOUND('',#1530,.T.);
#1076=FACE_OUTER_BOUND('',#1531,.T.);
#1077=FACE_OUTER_BOUND('',#1532,.T.);
#1078=FACE_OUTER_BOUND('',#1533,.T.);
#1079=FACE_OUTER_BOUND('',#1534,.T.);
#1080=FACE_OUTER_BOUND('',#1535,.T.);
#1081=FACE_OUTER_BOUND('',#1537,.T.);
#1082=FACE_OUTER_BOUND('',#1539,.T.);
#1083=FACE_OUTER_BOUND('',#1540,.T.);
#1084=FACE_OUTER_BOUND('',#1542,.T.);
#1085=EDGE_LOOP('',(#3961,#3962,#3963,#3964,#3965,#3966,#3967,#3968));
#1086=EDGE_LOOP('',(#3969));
#1087=EDGE_LOOP('',(#3970));
#1088=EDGE_LOOP('',(#3971));
#1089=EDGE_LOOP('',(#3972,#3973,#3974,#3975,#3976,#3977,#3978,#3979));
#1090=EDGE_LOOP('',(#3980,#3981,#3982,#3983));
#1091=EDGE_LOOP('',(#3984));
#1092=EDGE_LOOP('',(#3985));
#1093=EDGE_LOOP('',(#3986));
#1094=EDGE_LOOP('',(#3987));
#1095=EDGE_LOOP('',(#3988));
#1096=EDGE_LOOP('',(#3989));
#1097=EDGE_LOOP('',(#3990,#3991,#3992,#3993));
#1098=EDGE_LOOP('',(#3994,#3995,#3996,#3997));
#1099=EDGE_LOOP('',(#3998,#3999));
#1100=EDGE_LOOP('',(#4000,#4001));
#1101=EDGE_LOOP('',(#4002,#4003,#4004,#4005,#4006));
#1102=EDGE_LOOP('',(#4007,#4008,#4009,#4010,#4011,#4012,#4013,#4014,#4015));
#1103=EDGE_LOOP('',(#4016,#4017,#4018,#4019,#4020,#4021,#4022,#4023));
#1104=EDGE_LOOP('',(#4024));
#1105=EDGE_LOOP('',(#4025));
#1106=EDGE_LOOP('',(#4026));
#1107=EDGE_LOOP('',(#4027,#4028,#4029,#4030,#4031,#4032));
#1108=EDGE_LOOP('',(#4033,#4034,#4035,#4036,#4037,#4038));
#1109=EDGE_LOOP('',(#4039,#4040,#4041,#4042,#4043,#4044));
#1110=EDGE_LOOP('',(#4045,#4046,#4047,#4048,#4049,#4050));
#1111=EDGE_LOOP('',(#4051,#4052,#4053));
#1112=EDGE_LOOP('',(#4054,#4055,#4056));
#1113=EDGE_LOOP('',(#4057,#4058,#4059,#4060));
#1114=EDGE_LOOP('',(#4061,#4062,#4063,#4064));
#1115=EDGE_LOOP('',(#4065,#4066,#4067,#4068));
#1116=EDGE_LOOP('',(#4069,#4070,#4071,#4072));
#1117=EDGE_LOOP('',(#4073,#4074,#4075,#4076));
#1118=EDGE_LOOP('',(#4077,#4078,#4079,#4080));
#1119=EDGE_LOOP('',(#4081,#4082,#4083,#4084));
#1120=EDGE_LOOP('',(#4085,#4086,#4087,#4088,#4089,#4090,#4091,#4092));
#1121=EDGE_LOOP('',(#4093,#4094,#4095,#4096));
#1122=EDGE_LOOP('',(#4097,#4098,#4099));
#1123=EDGE_LOOP('',(#4100,#4101,#4102));
#1124=EDGE_LOOP('',(#4103,#4104,#4105,#4106,#4107,#4108));
#1125=EDGE_LOOP('',(#4109,#4110,#4111,#4112,#4113,#4114));
#1126=EDGE_LOOP('',(#4115,#4116,#4117,#4118));
#1127=EDGE_LOOP('',(#4119,#4120,#4121,#4122));
#1128=EDGE_LOOP('',(#4123,#4124,#4125,#4126));
#1129=EDGE_LOOP('',(#4127,#4128,#4129,#4130));
#1130=EDGE_LOOP('',(#4131,#4132,#4133,#4134));
#1131=EDGE_LOOP('',(#4135,#4136,#4137,#4138));
#1132=EDGE_LOOP('',(#4139,#4140,#4141,#4142));
#1133=EDGE_LOOP('',(#4143,#4144,#4145,#4146));
#1134=EDGE_LOOP('',(#4147,#4148,#4149,#4150,#4151,#4152,#4153));
#1135=EDGE_LOOP('',(#4154,#4155,#4156,#4157,#4158,#4159,#4160));
#1136=EDGE_LOOP('',(#4161,#4162,#4163,#4164,#4165));
#1137=EDGE_LOOP('',(#4166));
#1138=EDGE_LOOP('',(#4167));
#1139=EDGE_LOOP('',(#4168,#4169,#4170,#4171,#4172));
#1140=EDGE_LOOP('',(#4173));
#1141=EDGE_LOOP('',(#4174));
#1142=EDGE_LOOP('',(#4175,#4176,#4177,#4178,#4179));
#1143=EDGE_LOOP('',(#4180));
#1144=EDGE_LOOP('',(#4181));
#1145=EDGE_LOOP('',(#4182,#4183,#4184,#4185,#4186,#4187));
#1146=EDGE_LOOP('',(#4188));
#1147=EDGE_LOOP('',(#4189,#4190,#4191,#4192));
#1148=EDGE_LOOP('',(#4193,#4194,#4195,#4196));
#1149=EDGE_LOOP('',(#4197,#4198,#4199,#4200));
#1150=EDGE_LOOP('',(#4201,#4202,#4203,#4204));
#1151=EDGE_LOOP('',(#4205,#4206,#4207,#4208));
#1152=EDGE_LOOP('',(#4209,#4210,#4211,#4212));
#1153=EDGE_LOOP('',(#4213,#4214,#4215,#4216));
#1154=EDGE_LOOP('',(#4217,#4218,#4219,#4220));
#1155=EDGE_LOOP('',(#4221,#4222,#4223,#4224,#4225,#4226,#4227,#4228,#4229,
#4230,#4231));
#1156=EDGE_LOOP('',(#4232,#4233,#4234,#4235));
#1157=EDGE_LOOP('',(#4236,#4237,#4238,#4239));
#1158=EDGE_LOOP('',(#4240,#4241,#4242,#4243));
#1159=EDGE_LOOP('',(#4244,#4245,#4246,#4247));
#1160=EDGE_LOOP('',(#4248));
#1161=EDGE_LOOP('',(#4249));
#1162=EDGE_LOOP('',(#4250));
#1163=EDGE_LOOP('',(#4251));
#1164=EDGE_LOOP('',(#4252));
#1165=EDGE_LOOP('',(#4253));
#1166=EDGE_LOOP('',(#4254));
#1167=EDGE_LOOP('',(#4255));
#1168=EDGE_LOOP('',(#4256));
#1169=EDGE_LOOP('',(#4257,#4258,#4259));
#1170=EDGE_LOOP('',(#4260,#4261,#4262,#4263,#4264,#4265,#4266,#4267));
#1171=EDGE_LOOP('',(#4268,#4269));
#1172=EDGE_LOOP('',(#4270,#4271));
#1173=EDGE_LOOP('',(#4272,#4273,#4274,#4275));
#1174=EDGE_LOOP('',(#4276,#4277,#4278,#4279,#4280,#4281));
#1175=EDGE_LOOP('',(#4282,#4283,#4284,#4285,#4286,#4287));
#1176=EDGE_LOOP('',(#4288,#4289,#4290,#4291));
#1177=EDGE_LOOP('',(#4292,#4293,#4294,#4295,#4296,#4297,#4298,#4299));
#1178=EDGE_LOOP('',(#4300,#4301));
#1179=EDGE_LOOP('',(#4302,#4303));
#1180=EDGE_LOOP('',(#4304,#4305,#4306,#4307,#4308,#4309,#4310,#4311));
#1181=EDGE_LOOP('',(#4312,#4313));
#1182=EDGE_LOOP('',(#4314,#4315));
#1183=EDGE_LOOP('',(#4316,#4317,#4318,#4319,#4320,#4321,#4322,#4323));
#1184=EDGE_LOOP('',(#4324,#4325));
#1185=EDGE_LOOP('',(#4326,#4327));
#1186=EDGE_LOOP('',(#4328,#4329,#4330,#4331));
#1187=EDGE_LOOP('',(#4332,#4333,#4334,#4335,#4336,#4337));
#1188=EDGE_LOOP('',(#4338,#4339,#4340,#4341,#4342,#4343));
#1189=EDGE_LOOP('',(#4344,#4345,#4346,#4347));
#1190=EDGE_LOOP('',(#4348,#4349,#4350,#4351));
#1191=EDGE_LOOP('',(#4352,#4353,#4354,#4355,#4356,#4357));
#1192=EDGE_LOOP('',(#4358,#4359,#4360,#4361,#4362,#4363));
#1193=EDGE_LOOP('',(#4364,#4365,#4366,#4367));
#1194=EDGE_LOOP('',(#4368,#4369,#4370,#4371));
#1195=EDGE_LOOP('',(#4372,#4373,#4374,#4375,#4376,#4377));
#1196=EDGE_LOOP('',(#4378,#4379,#4380,#4381,#4382,#4383));
#1197=EDGE_LOOP('',(#4384,#4385,#4386,#4387));
#1198=EDGE_LOOP('',(#4388,#4389,#4390,#4391,#4392));
#1199=EDGE_LOOP('',(#4393,#4394,#4395,#4396,#4397));
#1200=EDGE_LOOP('',(#4398,#4399,#4400,#4401));
#1201=EDGE_LOOP('',(#4402));
#1202=EDGE_LOOP('',(#4403,#4404,#4405,#4406,#4407,#4408,#4409,#4410,#4411,
#4412,#4413));
#1203=EDGE_LOOP('',(#4414,#4415,#4416,#4417));
#1204=EDGE_LOOP('',(#4418,#4419,#4420,#4421));
#1205=EDGE_LOOP('',(#4422,#4423,#4424,#4425));
#1206=EDGE_LOOP('',(#4426,#4427,#4428,#4429));
#1207=EDGE_LOOP('',(#4430));
#1208=EDGE_LOOP('',(#4431));
#1209=EDGE_LOOP('',(#4432));
#1210=EDGE_LOOP('',(#4433));
#1211=EDGE_LOOP('',(#4434));
#1212=EDGE_LOOP('',(#4435));
#1213=EDGE_LOOP('',(#4436));
#1214=EDGE_LOOP('',(#4437));
#1215=EDGE_LOOP('',(#4438));
#1216=EDGE_LOOP('',(#4439));
#1217=EDGE_LOOP('',(#4440,#4441,#4442));
#1218=EDGE_LOOP('',(#4443,#4444,#4445,#4446,#4447,#4448,#4449,#4450));
#1219=EDGE_LOOP('',(#4451,#4452));
#1220=EDGE_LOOP('',(#4453,#4454));
#1221=EDGE_LOOP('',(#4455,#4456,#4457,#4458));
#1222=EDGE_LOOP('',(#4459,#4460,#4461,#4462,#4463,#4464));
#1223=EDGE_LOOP('',(#4465,#4466,#4467,#4468,#4469,#4470));
#1224=EDGE_LOOP('',(#4471,#4472,#4473,#4474));
#1225=EDGE_LOOP('',(#4475,#4476,#4477,#4478,#4479,#4480,#4481,#4482));
#1226=EDGE_LOOP('',(#4483,#4484));
#1227=EDGE_LOOP('',(#4485,#4486));
#1228=EDGE_LOOP('',(#4487,#4488,#4489,#4490,#4491,#4492,#4493,#4494));
#1229=EDGE_LOOP('',(#4495,#4496));
#1230=EDGE_LOOP('',(#4497,#4498));
#1231=EDGE_LOOP('',(#4499,#4500,#4501,#4502,#4503,#4504,#4505,#4506));
#1232=EDGE_LOOP('',(#4507,#4508));
#1233=EDGE_LOOP('',(#4509,#4510));
#1234=EDGE_LOOP('',(#4511,#4512,#4513,#4514));
#1235=EDGE_LOOP('',(#4515,#4516,#4517,#4518,#4519,#4520));
#1236=EDGE_LOOP('',(#4521,#4522,#4523,#4524,#4525,#4526));
#1237=EDGE_LOOP('',(#4527,#4528,#4529,#4530));
#1238=EDGE_LOOP('',(#4531,#4532,#4533,#4534));
#1239=EDGE_LOOP('',(#4535,#4536,#4537,#4538,#4539,#4540));
#1240=EDGE_LOOP('',(#4541,#4542,#4543,#4544,#4545,#4546));
#1241=EDGE_LOOP('',(#4547,#4548,#4549,#4550));
#1242=EDGE_LOOP('',(#4551,#4552,#4553,#4554));
#1243=EDGE_LOOP('',(#4555,#4556,#4557,#4558,#4559,#4560));
#1244=EDGE_LOOP('',(#4561,#4562,#4563,#4564,#4565,#4566));
#1245=EDGE_LOOP('',(#4567,#4568,#4569,#4570));
#1246=EDGE_LOOP('',(#4571,#4572,#4573,#4574,#4575));
#1247=EDGE_LOOP('',(#4576,#4577,#4578,#4579,#4580));
#1248=EDGE_LOOP('',(#4581,#4582,#4583,#4584));
#1249=EDGE_LOOP('',(#4585,#4586,#4587,#4588));
#1250=EDGE_LOOP('',(#4589,#4590,#4591,#4592));
#1251=EDGE_LOOP('',(#4593,#4594,#4595,#4596));
#1252=EDGE_LOOP('',(#4597,#4598,#4599,#4600));
#1253=EDGE_LOOP('',(#4601,#4602,#4603,#4604));
#1254=EDGE_LOOP('',(#4605,#4606,#4607,#4608));
#1255=EDGE_LOOP('',(#4609,#4610,#4611,#4612));
#1256=EDGE_LOOP('',(#4613,#4614,#4615,#4616));
#1257=EDGE_LOOP('',(#4617,#4618,#4619,#4620));
#1258=EDGE_LOOP('',(#4621,#4622,#4623,#4624));
#1259=EDGE_LOOP('',(#4625,#4626,#4627,#4628));
#1260=EDGE_LOOP('',(#4629,#4630,#4631,#4632));
#1261=EDGE_LOOP('',(#4633,#4634,#4635,#4636));
#1262=EDGE_LOOP('',(#4637,#4638,#4639,#4640));
#1263=EDGE_LOOP('',(#4641,#4642,#4643,#4644));
#1264=EDGE_LOOP('',(#4645,#4646,#4647,#4648));
#1265=EDGE_LOOP('',(#4649,#4650,#4651,#4652));
#1266=EDGE_LOOP('',(#4653,#4654,#4655,#4656));
#1267=EDGE_LOOP('',(#4657,#4658,#4659,#4660));
#1268=EDGE_LOOP('',(#4661,#4662,#4663,#4664));
#1269=EDGE_LOOP('',(#4665,#4666,#4667,#4668));
#1270=EDGE_LOOP('',(#4669,#4670,#4671,#4672,#4673,#4674,#4675,#4676,#4677,
#4678,#4679,#4680));
#1271=EDGE_LOOP('',(#4681));
#1272=EDGE_LOOP('',(#4682,#4683,#4684,#4685));
#1273=EDGE_LOOP('',(#4686,#4687,#4688,#4689));
#1274=EDGE_LOOP('',(#4690,#4691,#4692,#4693));
#1275=EDGE_LOOP('',(#4694,#4695,#4696,#4697,#4698,#4699,#4700,#4701,#4702,
#4703,#4704,#4705));
#1276=EDGE_LOOP('',(#4706));
#1277=EDGE_LOOP('',(#4707,#4708,#4709,#4710));
#1278=EDGE_LOOP('',(#4711,#4712,#4713,#4714));
#1279=EDGE_LOOP('',(#4715,#4716,#4717,#4718));
#1280=EDGE_LOOP('',(#4719,#4720,#4721,#4722,#4723,#4724,#4725,#4726,#4727,
#4728,#4729,#4730));
#1281=EDGE_LOOP('',(#4731));
#1282=EDGE_LOOP('',(#4732,#4733,#4734,#4735,#4736,#4737,#4738,#4739,#4740,
#4741));
#1283=EDGE_LOOP('',(#4742,#4743));
#1284=EDGE_LOOP('',(#4744,#4745));
#1285=EDGE_LOOP('',(#4746));
#1286=EDGE_LOOP('',(#4747));
#1287=EDGE_LOOP('',(#4748));
#1288=EDGE_LOOP('',(#4749));
#1289=EDGE_LOOP('',(#4750,#4751,#4752,#4753));
#1290=EDGE_LOOP('',(#4754));
#1291=EDGE_LOOP('',(#4755,#4756,#4757,#4758,#4759,#4760,#4761));
#1292=EDGE_LOOP('',(#4762));
#1293=EDGE_LOOP('',(#4763,#4764,#4765,#4766,#4767,#4768,#4769,#4770,#4771,
#4772,#4773,#4774));
#1294=EDGE_LOOP('',(#4775,#4776,#4777,#4778,#4779));
#1295=EDGE_LOOP('',(#4780,#4781,#4782,#4783,#4784,#4785,#4786));
#1296=EDGE_LOOP('',(#4787,#4788,#4789,#4790,#4791));
#1297=EDGE_LOOP('',(#4792,#4793,#4794,#4795,#4796));
#1298=EDGE_LOOP('',(#4797,#4798,#4799,#4800,#4801));
#1299=EDGE_LOOP('',(#4802));
#1300=EDGE_LOOP('',(#4803,#4804,#4805,#4806,#4807,#4808,#4809,#4810,#4811,
#4812,#4813,#4814));
#1301=EDGE_LOOP('',(#4815,#4816,#4817,#4818,#4819));
#1302=EDGE_LOOP('',(#4820));
#1303=EDGE_LOOP('',(#4821,#4822,#4823,#4824,#4825,#4826,#4827,#4828,#4829,
#4830,#4831,#4832));
#1304=EDGE_LOOP('',(#4833,#4834,#4835,#4836,#4837));
#1305=EDGE_LOOP('',(#4838,#4839,#4840,#4841,#4842));
#1306=EDGE_LOOP('',(#4843,#4844,#4845,#4846,#4847));
#1307=EDGE_LOOP('',(#4848,#4849,#4850,#4851,#4852));
#1308=EDGE_LOOP('',(#4853,#4854,#4855,#4856,#4857));
#1309=EDGE_LOOP('',(#4858));
#1310=EDGE_LOOP('',(#4859,#4860,#4861,#4862,#4863,#4864,#4865,#4866,#4867,
#4868));
#1311=EDGE_LOOP('',(#4869,#4870));
#1312=EDGE_LOOP('',(#4871,#4872));
#1313=EDGE_LOOP('',(#4873,#4874,#4875,#4876));
#1314=EDGE_LOOP('',(#4877,#4878,#4879,#4880));
#1315=EDGE_LOOP('',(#4881,#4882,#4883,#4884));
#1316=EDGE_LOOP('',(#4885,#4886,#4887,#4888));
#1317=EDGE_LOOP('',(#4889,#4890,#4891,#4892));
#1318=EDGE_LOOP('',(#4893,#4894,#4895,#4896));
#1319=EDGE_LOOP('',(#4897,#4898,#4899,#4900));
#1320=EDGE_LOOP('',(#4901,#4902,#4903,#4904));
#1321=EDGE_LOOP('',(#4905,#4906,#4907,#4908));
#1322=EDGE_LOOP('',(#4909,#4910,#4911,#4912));
#1323=EDGE_LOOP('',(#4913,#4914,#4915,#4916));
#1324=EDGE_LOOP('',(#4917,#4918,#4919,#4920));
#1325=EDGE_LOOP('',(#4921,#4922,#4923,#4924));
#1326=EDGE_LOOP('',(#4925,#4926,#4927,#4928));
#1327=EDGE_LOOP('',(#4929,#4930,#4931,#4932));
#1328=EDGE_LOOP('',(#4933,#4934,#4935,#4936));
#1329=EDGE_LOOP('',(#4937,#4938,#4939,#4940));
#1330=EDGE_LOOP('',(#4941,#4942,#4943,#4944));
#1331=EDGE_LOOP('',(#4945,#4946,#4947,#4948));
#1332=EDGE_LOOP('',(#4949,#4950,#4951,#4952));
#1333=EDGE_LOOP('',(#4953,#4954,#4955,#4956));
#1334=EDGE_LOOP('',(#4957,#4958,#4959,#4960));
#1335=EDGE_LOOP('',(#4961,#4962,#4963,#4964));
#1336=EDGE_LOOP('',(#4965,#4966,#4967,#4968));
#1337=EDGE_LOOP('',(#4969,#4970,#4971,#4972));
#1338=EDGE_LOOP('',(#4973,#4974,#4975,#4976));
#1339=EDGE_LOOP('',(#4977,#4978,#4979,#4980));
#1340=EDGE_LOOP('',(#4981,#4982,#4983,#4984));
#1341=EDGE_LOOP('',(#4985));
#1342=EDGE_LOOP('',(#4986));
#1343=EDGE_LOOP('',(#4987));
#1344=EDGE_LOOP('',(#4988));
#1345=EDGE_LOOP('',(#4989,#4990,#4991,#4992));
#1346=EDGE_LOOP('',(#4993,#4994,#4995,#4996));
#1347=EDGE_LOOP('',(#4997));
#1348=EDGE_LOOP('',(#4998));
#1349=EDGE_LOOP('',(#4999,#5000,#5001,#5002));
#1350=EDGE_LOOP('',(#5003,#5004,#5005,#5006));
#1351=EDGE_LOOP('',(#5007));
#1352=EDGE_LOOP('',(#5008));
#1353=EDGE_LOOP('',(#5009));
#1354=EDGE_LOOP('',(#5010));
#1355=EDGE_LOOP('',(#5011,#5012,#5013,#5014));
#1356=EDGE_LOOP('',(#5015,#5016,#5017,#5018));
#1357=EDGE_LOOP('',(#5019));
#1358=EDGE_LOOP('',(#5020));
#1359=EDGE_LOOP('',(#5021,#5022,#5023,#5024));
#1360=EDGE_LOOP('',(#5025,#5026,#5027,#5028));
#1361=EDGE_LOOP('',(#5029));
#1362=EDGE_LOOP('',(#5030));
#1363=EDGE_LOOP('',(#5031));
#1364=EDGE_LOOP('',(#5032));
#1365=EDGE_LOOP('',(#5033,#5034,#5035,#5036));
#1366=EDGE_LOOP('',(#5037,#5038,#5039,#5040));
#1367=EDGE_LOOP('',(#5041));
#1368=EDGE_LOOP('',(#5042));
#1369=EDGE_LOOP('',(#5043,#5044,#5045,#5046));
#1370=EDGE_LOOP('',(#5047,#5048,#5049,#5050));
#1371=EDGE_LOOP('',(#5051));
#1372=EDGE_LOOP('',(#5052));
#1373=EDGE_LOOP('',(#5053));
#1374=EDGE_LOOP('',(#5054));
#1375=EDGE_LOOP('',(#5055,#5056,#5057,#5058));
#1376=EDGE_LOOP('',(#5059,#5060,#5061,#5062));
#1377=EDGE_LOOP('',(#5063));
#1378=EDGE_LOOP('',(#5064));
#1379=EDGE_LOOP('',(#5065,#5066,#5067,#5068));
#1380=EDGE_LOOP('',(#5069,#5070,#5071,#5072));
#1381=EDGE_LOOP('',(#5073,#5074,#5075,#5076));
#1382=EDGE_LOOP('',(#5077,#5078,#5079,#5080));
#1383=EDGE_LOOP('',(#5081,#5082,#5083,#5084,#5085,#5086));
#1384=EDGE_LOOP('',(#5087,#5088,#5089,#5090,#5091));
#1385=EDGE_LOOP('',(#5092,#5093,#5094,#5095,#5096));
#1386=EDGE_LOOP('',(#5097,#5098,#5099,#5100));
#1387=EDGE_LOOP('',(#5101,#5102,#5103,#5104));
#1388=EDGE_LOOP('',(#5105,#5106,#5107,#5108,#5109,#5110));
#1389=EDGE_LOOP('',(#5111,#5112,#5113,#5114,#5115));
#1390=EDGE_LOOP('',(#5116,#5117,#5118,#5119,#5120));
#1391=EDGE_LOOP('',(#5121,#5122,#5123,#5124));
#1392=EDGE_LOOP('',(#5125,#5126,#5127,#5128,#5129,#5130));
#1393=EDGE_LOOP('',(#5131,#5132,#5133,#5134,#5135));
#1394=EDGE_LOOP('',(#5136,#5137,#5138,#5139,#5140));
#1395=EDGE_LOOP('',(#5141,#5142,#5143,#5144));
#1396=EDGE_LOOP('',(#5145,#5146,#5147,#5148));
#1397=EDGE_LOOP('',(#5149,#5150,#5151,#5152));
#1398=EDGE_LOOP('',(#5153));
#1399=EDGE_LOOP('',(#5154,#5155,#5156,#5157,#5158,#5159,#5160,#5161,#5162,
#5163,#5164,#5165));
#1400=EDGE_LOOP('',(#5166));
#1401=EDGE_LOOP('',(#5167,#5168,#5169,#5170,#5171,#5172,#5173,#5174,#5175,
#5176,#5177,#5178));
#1402=EDGE_LOOP('',(#5179,#5180,#5181,#5182));
#1403=EDGE_LOOP('',(#5183,#5184,#5185,#5186,#5187,#5188,#5189,#5190,#5191,
#5192,#5193,#5194));
#1404=EDGE_LOOP('',(#5195));
#1405=EDGE_LOOP('',(#5196,#5197,#5198,#5199,#5200,#5201,#5202,#5203,#5204,
#5205,#5206,#5207));
#1406=EDGE_LOOP('',(#5208));
#1407=EDGE_LOOP('',(#5209));
#1408=EDGE_LOOP('',(#5210,#5211,#5212,#5213,#5214,#5215,#5216,#5217));
#1409=EDGE_LOOP('',(#5218));
#1410=EDGE_LOOP('',(#5219));
#1411=EDGE_LOOP('',(#5220,#5221,#5222,#5223,#5224,#5225));
#1412=EDGE_LOOP('',(#5226));
#1413=EDGE_LOOP('',(#5227));
#1414=EDGE_LOOP('',(#5228,#5229,#5230,#5231,#5232,#5233));
#1415=EDGE_LOOP('',(#5234));
#1416=EDGE_LOOP('',(#5235));
#1417=EDGE_LOOP('',(#5236,#5237,#5238,#5239,#5240,#5241));
#1418=EDGE_LOOP('',(#5242));
#1419=EDGE_LOOP('',(#5243));
#1420=EDGE_LOOP('',(#5244,#5245,#5246,#5247));
#1421=EDGE_LOOP('',(#5248));
#1422=EDGE_LOOP('',(#5249));
#1423=EDGE_LOOP('',(#5250,#5251,#5252,#5253));
#1424=EDGE_LOOP('',(#5254));
#1425=EDGE_LOOP('',(#5255));
#1426=EDGE_LOOP('',(#5256,#5257,#5258,#5259));
#1427=EDGE_LOOP('',(#5260,#5261,#5262,#5263));
#1428=EDGE_LOOP('',(#5264,#5265));
#1429=EDGE_LOOP('',(#5266,#5267));
#1430=EDGE_LOOP('',(#5268,#5269));
#1431=EDGE_LOOP('',(#5270,#5271));
#1432=EDGE_LOOP('',(#5272,#5273));
#1433=EDGE_LOOP('',(#5274,#5275));
#1434=EDGE_LOOP('',(#5276,#5277));
#1435=EDGE_LOOP('',(#5278,#5279));
#1436=EDGE_LOOP('',(#5280,#5281));
#1437=EDGE_LOOP('',(#5282,#5283));
#1438=EDGE_LOOP('',(#5284,#5285));
#1439=EDGE_LOOP('',(#5286,#5287));
#1440=EDGE_LOOP('',(#5288));
#1441=EDGE_LOOP('',(#5289));
#1442=EDGE_LOOP('',(#5290));
#1443=EDGE_LOOP('',(#5291,#5292,#5293,#5294));
#1444=EDGE_LOOP('',(#5295,#5296,#5297,#5298,#5299));
#1445=EDGE_LOOP('',(#5300,#5301,#5302,#5303,#5304));
#1446=EDGE_LOOP('',(#5305,#5306,#5307,#5308,#5309));
#1447=EDGE_LOOP('',(#5310,#5311,#5312,#5313,#5314));
#1448=EDGE_LOOP('',(#5315));
#1449=EDGE_LOOP('',(#5316));
#1450=EDGE_LOOP('',(#5317,#5318,#5319,#5320,#5321,#5322,#5323,#5324));
#1451=EDGE_LOOP('',(#5325));
#1452=EDGE_LOOP('',(#5326));
#1453=EDGE_LOOP('',(#5327,#5328,#5329,#5330,#5331,#5332,#5333,#5334));
#1454=EDGE_LOOP('',(#5335));
#1455=EDGE_LOOP('',(#5336));
#1456=EDGE_LOOP('',(#5337,#5338,#5339,#5340,#5341,#5342));
#1457=EDGE_LOOP('',(#5343));
#1458=EDGE_LOOP('',(#5344));
#1459=EDGE_LOOP('',(#5345,#5346,#5347,#5348,#5349,#5350));
#1460=EDGE_LOOP('',(#5351));
#1461=EDGE_LOOP('',(#5352));
#1462=EDGE_LOOP('',(#5353,#5354,#5355,#5356,#5357,#5358));
#1463=EDGE_LOOP('',(#5359));
#1464=EDGE_LOOP('',(#5360));
#1465=EDGE_LOOP('',(#5361,#5362,#5363,#5364,#5365,#5366));
#1466=EDGE_LOOP('',(#5367));
#1467=EDGE_LOOP('',(#5368));
#1468=EDGE_LOOP('',(#5369,#5370,#5371,#5372,#5373,#5374));
#1469=EDGE_LOOP('',(#5375));
#1470=EDGE_LOOP('',(#5376));
#1471=EDGE_LOOP('',(#5377,#5378,#5379,#5380,#5381,#5382));
#1472=EDGE_LOOP('',(#5383,#5384,#5385,#5386,#5387));
#1473=EDGE_LOOP('',(#5388,#5389,#5390,#5391,#5392));
#1474=EDGE_LOOP('',(#5393,#5394,#5395,#5396,#5397));
#1475=EDGE_LOOP('',(#5398,#5399,#5400,#5401,#5402));
#1476=EDGE_LOOP('',(#5403,#5404,#5405,#5406,#5407));
#1477=EDGE_LOOP('',(#5408,#5409,#5410,#5411,#5412));
#1478=EDGE_LOOP('',(#5413,#5414,#5415,#5416,#5417));
#1479=EDGE_LOOP('',(#5418,#5419,#5420,#5421,#5422));
#1480=EDGE_LOOP('',(#5423));
#1481=EDGE_LOOP('',(#5424));
#1482=EDGE_LOOP('',(#5425,#5426,#5427,#5428));
#1483=EDGE_LOOP('',(#5429));
#1484=EDGE_LOOP('',(#5430));
#1485=EDGE_LOOP('',(#5431,#5432,#5433,#5434));
#1486=EDGE_LOOP('',(#5435));
#1487=EDGE_LOOP('',(#5436));
#1488=EDGE_LOOP('',(#5437,#5438,#5439,#5440));
#1489=EDGE_LOOP('',(#5441));
#1490=EDGE_LOOP('',(#5442));
#1491=EDGE_LOOP('',(#5443,#5444,#5445,#5446));
#1492=EDGE_LOOP('',(#5447));
#1493=EDGE_LOOP('',(#5448));
#1494=EDGE_LOOP('',(#5449,#5450,#5451,#5452));
#1495=EDGE_LOOP('',(#5453));
#1496=EDGE_LOOP('',(#5454));
#1497=EDGE_LOOP('',(#5455,#5456,#5457,#5458));
#1498=EDGE_LOOP('',(#5459));
#1499=EDGE_LOOP('',(#5460));
#1500=EDGE_LOOP('',(#5461,#5462,#5463,#5464));
#1501=EDGE_LOOP('',(#5465));
#1502=EDGE_LOOP('',(#5466));
#1503=EDGE_LOOP('',(#5467,#5468,#5469,#5470));
#1504=EDGE_LOOP('',(#5471,#5472,#5473,#5474));
#1505=EDGE_LOOP('',(#5475,#5476,#5477,#5478));
#1506=EDGE_LOOP('',(#5479,#5480,#5481,#5482,#5483,#5484,#5485));
#1507=EDGE_LOOP('',(#5486,#5487,#5488,#5489,#5490,#5491,#5492));
#1508=EDGE_LOOP('',(#5493,#5494,#5495,#5496));
#1509=EDGE_LOOP('',(#5497,#5498,#5499,#5500));
#1510=EDGE_LOOP('',(#5501,#5502,#5503,#5504));
#1511=EDGE_LOOP('',(#5505,#5506,#5507,#5508));
#1512=EDGE_LOOP('',(#5509,#5510,#5511,#5512));
#1513=EDGE_LOOP('',(#5513,#5514,#5515,#5516,#5517,#5518,#5519));
#1514=EDGE_LOOP('',(#5520,#5521,#5522,#5523,#5524,#5525,#5526));
#1515=EDGE_LOOP('',(#5527,#5528,#5529,#5530));
#1516=EDGE_LOOP('',(#5531,#5532,#5533,#5534));
#1517=EDGE_LOOP('',(#5535,#5536,#5537,#5538));
#1518=EDGE_LOOP('',(#5539,#5540,#5541,#5542));
#1519=EDGE_LOOP('',(#5543,#5544,#5545,#5546));
#1520=EDGE_LOOP('',(#5547,#5548,#5549,#5550,#5551,#5552,#5553));
#1521=EDGE_LOOP('',(#5554,#5555,#5556,#5557,#5558,#5559,#5560));
#1522=EDGE_LOOP('',(#5561,#5562,#5563,#5564));
#1523=EDGE_LOOP('',(#5565,#5566,#5567,#5568));
#1524=EDGE_LOOP('',(#5569,#5570,#5571,#5572));
#1525=EDGE_LOOP('',(#5573,#5574,#5575,#5576));
#1526=EDGE_LOOP('',(#5577,#5578,#5579,#5580));
#1527=EDGE_LOOP('',(#5581,#5582,#5583,#5584));
#1528=EDGE_LOOP('',(#5585,#5586,#5587,#5588));
#1529=EDGE_LOOP('',(#5589,#5590,#5591,#5592));
#1530=EDGE_LOOP('',(#5593,#5594,#5595,#5596));
#1531=EDGE_LOOP('',(#5597,#5598,#5599,#5600));
#1532=EDGE_LOOP('',(#5601,#5602,#5603,#5604));
#1533=EDGE_LOOP('',(#5605,#5606,#5607,#5608));
#1534=EDGE_LOOP('',(#5609,#5610,#5611,#5612));
#1535=EDGE_LOOP('',(#5613));
#1536=EDGE_LOOP('',(#5614));
#1537=EDGE_LOOP('',(#5615));
#1538=EDGE_LOOP('',(#5616));
#1539=EDGE_LOOP('',(#5617,#5618,#5619,#5620));
#1540=EDGE_LOOP('',(#5621));
#1541=EDGE_LOOP('',(#5622));
#1542=EDGE_LOOP('',(#5623,#5624,#5625,#5626));
#1543=CIRCLE('',#6261,65.8399949356644);
#1544=CIRCLE('',#6262,3.99999999999999);
#1545=CIRCLE('',#6263,15.9631510575949);
#1546=CIRCLE('',#6264,3.99999999999999);
#1547=CIRCLE('',#6266,109.542028553823);
#1548=CIRCLE('',#6267,65.8399949356645);
#1549=CIRCLE('',#6268,109.542028553823);
#1550=CIRCLE('',#6269,37.);
#1551=CIRCLE('',#6270,109.542028553823);
#1552=CIRCLE('',#6271,65.8399949356644);
#1553=CIRCLE('',#6272,109.542028553823);
#1554=CIRCLE('',#6273,37.);
#1555=CIRCLE('',#6274,3.99999999999999);
#1556=CIRCLE('',#6275,15.9631510575949);
#1557=CIRCLE('',#6276,3.99999999999999);
#1558=CIRCLE('',#6277,3.99999999999999);
#1559=CIRCLE('',#6278,15.9631510575949);
#1560=CIRCLE('',#6279,3.99999999999999);
#1561=CIRCLE('',#6281,14.);
#1562=CIRCLE('',#6282,14.);
#1563=CIRCLE('',#6284,13.897506768291);
#1564=CIRCLE('',#6286,50.0401279512714);
#1565=CIRCLE('',#6287,50.0401279512714);
#1566=CIRCLE('',#6289,65.8399949356645);
#1567=CIRCLE('',#6290,3.99999999999999);
#1568=CIRCLE('',#6291,15.9631510575949);
#1569=CIRCLE('',#6292,3.99999999999999);
#1570=CIRCLE('',#6294,50.0401279512714);
#1571=CIRCLE('',#6296,50.0401279512714);
#1572=CIRCLE('',#6313,17.5);
#1573=CIRCLE('',#6314,17.5);
#1574=CIRCLE('',#6316,17.5);
#1575=CIRCLE('',#6317,17.5);
#1576=CIRCLE('',#6319,17.5);
#1577=CIRCLE('',#6321,13.897506768291);
#1578=CIRCLE('',#6323,17.5);
#1579=CIRCLE('',#6327,20.);
#1580=CIRCLE('',#6340,20.5);
#1581=CIRCLE('',#6341,20.5);
#1582=CIRCLE('',#6342,20.5);
#1583=CIRCLE('',#6343,20.5);
#1584=CIRCLE('',#6344,20.5);
#1585=CIRCLE('',#6345,20.5);
#1586=CIRCLE('',#6346,20.5);
#1587=CIRCLE('',#6347,20.5);
#1588=CIRCLE('',#6348,20.5);
#1589=CIRCLE('',#6349,20.5);
#1590=CIRCLE('',#6350,20.5);
#1591=CIRCLE('',#6351,20.5);
#1592=CIRCLE('',#6353,19.5);
#1593=CIRCLE('',#6355,19.5);
#1594=CIRCLE('',#6356,17.5);
#1595=CIRCLE('',#6358,1.02425693042952);
#1596=CIRCLE('',#6359,1.02425693042952);
#1597=CIRCLE('',#6361,21.5);
#1598=CIRCLE('',#6363,21.5);
#1599=CIRCLE('',#6369,1.02425693042952);
#1600=CIRCLE('',#6370,1.02425693042952);
#1601=CIRCLE('',#6372,21.5);
#1602=CIRCLE('',#6374,21.5);
#1603=CIRCLE('',#6376,1.02425693042952);
#1604=CIRCLE('',#6377,1.02425693042952);
#1605=CIRCLE('',#6379,21.5);
#1606=CIRCLE('',#6381,21.5);
#1607=CIRCLE('',#6383,1.02425693042952);
#1608=CIRCLE('',#6384,1.02425693042952);
#1609=CIRCLE('',#6386,21.5);
#1610=CIRCLE('',#6388,21.5);
#1611=CIRCLE('',#6402,1.);
#1612=CIRCLE('',#6404,1.);
#1613=CIRCLE('',#6406,17.5);
#1614=CIRCLE('',#6410,20.5);
#1615=CIRCLE('',#6411,20.5);
#1616=CIRCLE('',#6412,20.5);
#1617=CIRCLE('',#6413,20.5);
#1618=CIRCLE('',#6414,20.5);
#1619=CIRCLE('',#6415,20.5);
#1620=CIRCLE('',#6416,20.5);
#1621=CIRCLE('',#6417,20.5);
#1622=CIRCLE('',#6418,20.5);
#1623=CIRCLE('',#6419,20.5);
#1624=CIRCLE('',#6420,20.5);
#1625=CIRCLE('',#6421,20.5);
#1626=CIRCLE('',#6423,19.5);
#1627=CIRCLE('',#6424,17.5);
#1628=CIRCLE('',#6426,19.5);
#1629=CIRCLE('',#6427,17.5);
#1630=CIRCLE('',#6429,1.02425693042952);
#1631=CIRCLE('',#6430,1.02425693042952);
#1632=CIRCLE('',#6432,21.5);
#1633=CIRCLE('',#6434,21.5);
#1634=CIRCLE('',#6440,1.02425693042952);
#1635=CIRCLE('',#6441,1.02425693042952);
#1636=CIRCLE('',#6443,21.5);
#1637=CIRCLE('',#6445,21.5);
#1638=CIRCLE('',#6447,1.02425693042952);
#1639=CIRCLE('',#6448,1.02425693042952);
#1640=CIRCLE('',#6450,21.5);
#1641=CIRCLE('',#6452,21.5);
#1642=CIRCLE('',#6454,1.02425693042952);
#1643=CIRCLE('',#6455,1.02425693042952);
#1644=CIRCLE('',#6457,21.5);
#1645=CIRCLE('',#6459,21.5);
#1646=CIRCLE('',#6473,1.);
#1647=CIRCLE('',#6475,1.);
#1648=CIRCLE('',#6480,13.0000000000012);
#1649=CIRCLE('',#6481,10.9999999999984);
#1650=CIRCLE('',#6484,10.9999999999984);
#1651=CIRCLE('',#6487,13.);
#1652=CIRCLE('',#6490,13.0000000000012);
#1653=CIRCLE('',#6491,10.9999999999984);
#1654=CIRCLE('',#6494,10.9999999999984);
#1655=CIRCLE('',#6497,13.);
#1656=CIRCLE('',#6500,13.0000000000012);
#1657=CIRCLE('',#6501,10.9999999999984);
#1658=CIRCLE('',#6504,10.9999999999984);
#1659=CIRCLE('',#6507,13.);
#1660=CIRCLE('',#6510,15.);
#1661=CIRCLE('',#6511,15.);
#1662=CIRCLE('',#6513,15.);
#1663=CIRCLE('',#6514,15.);
#1664=CIRCLE('',#6516,15.);
#1665=CIRCLE('',#6517,15.);
#1666=CIRCLE('',#6519,13.);
#1667=CIRCLE('',#6521,15.);
#1668=CIRCLE('',#6522,15.);
#1669=CIRCLE('',#6524,15.);
#1670=CIRCLE('',#6525,15.);
#1671=CIRCLE('',#6527,15.);
#1672=CIRCLE('',#6528,15.);
#1673=CIRCLE('',#6530,13.);
#1674=CIRCLE('',#6532,15.);
#1675=CIRCLE('',#6533,15.);
#1676=CIRCLE('',#6535,15.);
#1677=CIRCLE('',#6536,15.);
#1678=CIRCLE('',#6538,15.);
#1679=CIRCLE('',#6539,15.);
#1680=CIRCLE('',#6541,13.);
#1681=CIRCLE('',#6543,28.1634258170599);
#1682=CIRCLE('',#6544,28.1634258170599);
#1683=CIRCLE('',#6546,23.1634258170599);
#1684=CIRCLE('',#6548,20.);
#1685=CIRCLE('',#6550,23.1634258170599);
#1686=CIRCLE('',#6553,15.);
#1687=CIRCLE('',#6555,17.);
#1688=CIRCLE('',#6557,17.);
#1689=CIRCLE('',#6558,17.);
#1690=CIRCLE('',#6562,15.);
#1691=CIRCLE('',#6564,15.);
#1692=CIRCLE('',#6566,17.);
#1693=CIRCLE('',#6568,17.);
#1694=CIRCLE('',#6569,17.);
#1695=CIRCLE('',#6571,17.);
#1696=CIRCLE('',#6573,17.);
#1697=CIRCLE('',#6574,17.);
#1698=CIRCLE('',#6580,20.);
#1699=CIRCLE('',#6611,3.99999999999999);
#1700=CIRCLE('',#6612,3.99999999999999);
#1701=CIRCLE('',#6614,3.49999999999999);
#1702=CIRCLE('',#6616,1.8);
#1703=CIRCLE('',#6618,0.899999999999989);
#1704=CIRCLE('',#6619,0.899999999999988);
#1705=CIRCLE('',#6622,3.49999999999999);
#1706=CIRCLE('',#6626,4.00000000000001);
#1707=CIRCLE('',#6627,4.00000000000001);
#1708=CIRCLE('',#6629,3.50000000000001);
#1709=CIRCLE('',#6631,1.8);
#1710=CIRCLE('',#6633,0.899999999999997);
#1711=CIRCLE('',#6634,0.899999999999995);
#1712=CIRCLE('',#6637,3.50000000000001);
#1713=CIRCLE('',#6641,4.);
#1714=CIRCLE('',#6642,4.);
#1715=CIRCLE('',#6644,3.49999999999993);
#1716=CIRCLE('',#6646,1.80000000000001);
#1717=CIRCLE('',#6648,0.900000000000014);
#1718=CIRCLE('',#6649,0.899999999999985);
#1719=CIRCLE('',#6652,3.49999999999993);
#1720=CIRCLE('',#6656,4.00000000000013);
#1721=CIRCLE('',#6657,4.00000000000013);
#1722=CIRCLE('',#6659,3.50000000000012);
#1723=CIRCLE('',#6661,1.8);
#1724=CIRCLE('',#6663,0.89999999999999);
#1725=CIRCLE('',#6664,0.899999999999984);
#1726=CIRCLE('',#6667,3.50000000000012);
#1727=CIRCLE('',#6671,15.);
#1728=CIRCLE('',#6672,15.);
#1729=CIRCLE('',#6674,15.);
#1730=CIRCLE('',#6675,15.);
#1731=CIRCLE('',#6677,15.);
#1732=CIRCLE('',#6678,15.);
#1733=CIRCLE('',#6684,15.);
#1734=CIRCLE('',#6685,15.);
#1735=CIRCLE('',#6695,15.);
#1736=CIRCLE('',#6696,15.);
#1737=CIRCLE('',#6698,15.);
#1738=CIRCLE('',#6699,15.);
#1739=CIRCLE('',#6701,17.);
#1740=CIRCLE('',#6702,14.5);
#1741=CIRCLE('',#6703,14.5);
#1742=CIRCLE('',#6704,14.5);
#1743=CIRCLE('',#6706,17.);
#1744=CIRCLE('',#6709,12.9999999999984);
#1745=CIRCLE('',#6711,14.5);
#1746=CIRCLE('',#6712,14.5);
#1747=CIRCLE('',#6713,14.5);
#1748=CIRCLE('',#6715,4.00000000000012);
#1749=CIRCLE('',#6716,3.50000000000012);
#1750=CIRCLE('',#6719,4.00000000000001);
#1751=CIRCLE('',#6720,3.5);
#1752=CIRCLE('',#6723,4.00000000000001);
#1753=CIRCLE('',#6724,3.49999999999992);
#1754=CIRCLE('',#6727,4.);
#1755=CIRCLE('',#6728,3.49999999999998);
#1756=CIRCLE('',#6731,3.50000000000012);
#1757=CIRCLE('',#6732,2.80000000000012);
#1758=CIRCLE('',#6735,3.5);
#1759=CIRCLE('',#6736,2.79999999999998);
#1760=CIRCLE('',#6739,3.49999999999992);
#1761=CIRCLE('',#6740,2.79999999999991);
#1762=CIRCLE('',#6743,12.9999999999984);
#1763=CIRCLE('',#6746,3.49999999999998);
#1764=CIRCLE('',#6747,2.79999999999999);
#1765=CIRCLE('',#6754,4.00000000000012);
#1766=CIRCLE('',#6755,3.50000000000012);
#1767=CIRCLE('',#6758,4.00000000000012);
#1768=CIRCLE('',#6759,3.50000000000012);
#1769=CIRCLE('',#6762,4.00000000000001);
#1770=CIRCLE('',#6763,3.5);
#1771=CIRCLE('',#6766,4.00000000000001);
#1772=CIRCLE('',#6767,3.5);
#1773=CIRCLE('',#6770,4.00000000000001);
#1774=CIRCLE('',#6771,3.49999999999992);
#1775=CIRCLE('',#6774,4.00000000000001);
#1776=CIRCLE('',#6775,3.49999999999992);
#1777=CIRCLE('',#6778,4.);
#1778=CIRCLE('',#6779,3.49999999999998);
#1779=CIRCLE('',#6782,4.);
#1780=CIRCLE('',#6783,3.49999999999998);
#1781=CIRCLE('',#6786,2.80000000000012);
#1782=CIRCLE('',#6788,2.80000000000012);
#1783=CIRCLE('',#6790,2.79999999999998);
#1784=CIRCLE('',#6792,2.79999999999998);
#1785=CIRCLE('',#6794,2.79999999999991);
#1786=CIRCLE('',#6796,2.79999999999991);
#1787=CIRCLE('',#6798,2.79999999999999);
#1788=CIRCLE('',#6800,2.79999999999999);
#1789=CIRCLE('',#6802,3.50000000000012);
#1790=CIRCLE('',#6805,3.50000000000012);
#1791=CIRCLE('',#6808,3.5);
#1792=CIRCLE('',#6811,3.5);
#1793=CIRCLE('',#6814,3.49999999999992);
#1794=CIRCLE('',#6817,3.49999999999992);
#1795=CIRCLE('',#6820,3.49999999999998);
#1796=CIRCLE('',#6823,3.49999999999998);
#1797=CIRCLE('',#6891,16.);
#1798=CIRCLE('',#6892,15.8253961525413);
#1799=CIRCLE('',#6894,12.);
#1800=CIRCLE('',#6896,14.);
#1801=CIRCLE('',#6898,14.);
#1802=CIRCLE('',#6900,12.);
#1803=LINE('',#8598,#2191);
#1804=LINE('',#8600,#2192);
#1805=LINE('',#8602,#2193);
#1806=LINE('',#8604,#2194);
#1807=LINE('',#8606,#2195);
#1808=LINE('',#8610,#2196);
#1809=LINE('',#8611,#2197);
#1810=LINE('',#8637,#2198);
#1811=LINE('',#8639,#2199);
#1812=LINE('',#8641,#2200);
#1813=LINE('',#8642,#2201);
#1814=LINE('',#8657,#2202);
#1815=LINE('',#8659,#2203);
#1816=LINE('',#8661,#2204);
#1817=LINE('',#8662,#2205);
#1818=LINE('',#8667,#2206);
#1819=LINE('',#8828,#2207);
#1820=LINE('',#8832,#2208);
#1821=LINE('',#8872,#2209);
#1822=LINE('',#8876,#2210);
#1823=LINE('',#8904,#2211);
#1824=LINE('',#8909,#2212);
#1825=LINE('',#8911,#2213);
#1826=LINE('',#8913,#2214);
#1827=LINE('',#8915,#2215);
#1828=LINE('',#8919,#2216);
#1829=LINE('',#8921,#2217);
#1830=LINE('',#8922,#2218);
#1831=LINE('',#8933,#2219);
#1832=LINE('',#8934,#2220);
#1833=LINE('',#9120,#2221);
#1834=LINE('',#9122,#2222);
#1835=LINE('',#9307,#2223);
#1836=LINE('',#9308,#2224);
#1837=LINE('',#9314,#2225);
#1838=LINE('',#9315,#2226);
#1839=LINE('',#9326,#2227);
#1840=LINE('',#9329,#2228);
#1841=LINE('',#9385,#2229);
#1842=LINE('',#9386,#2230);
#1843=LINE('',#9436,#2231);
#1844=LINE('',#9437,#2232);
#1845=LINE('',#9553,#2233);
#1846=LINE('',#9625,#2234);
#1847=LINE('',#9731,#2235);
#1848=LINE('',#9733,#2236);
#1849=LINE('',#9768,#2237);
#1850=LINE('',#9769,#2238);
#1851=LINE('',#9779,#2239);
#1852=LINE('',#9781,#2240);
#1853=LINE('',#9783,#2241);
#1854=LINE('',#9785,#2242);
#1855=LINE('',#9834,#2243);
#1856=LINE('',#9883,#2244);
#1857=LINE('',#9998,#2245);
#1858=LINE('',#10063,#2246);
#1859=LINE('',#10158,#2247);
#1860=LINE('',#10165,#2248);
#1861=LINE('',#10169,#2249);
#1862=LINE('',#10174,#2250);
#1863=LINE('',#10179,#2251);
#1864=LINE('',#10181,#2252);
#1865=LINE('',#10183,#2253);
#1866=LINE('',#10185,#2254);
#1867=LINE('',#10187,#2255);
#1868=LINE('',#10189,#2256);
#1869=LINE('',#10197,#2257);
#1870=LINE('',#10231,#2258);
#1871=LINE('',#10262,#2259);
#1872=LINE('',#10266,#2260);
#1873=LINE('',#10270,#2261);
#1874=LINE('',#10274,#2262);
#1875=LINE('',#10278,#2263);
#1876=LINE('',#10282,#2264);
#1877=LINE('',#10286,#2265);
#1878=LINE('',#10290,#2266);
#1879=LINE('',#10507,#2267);
#1880=LINE('',#10525,#2268);
#1881=LINE('',#10592,#2269);
#1882=LINE('',#10610,#2270);
#1883=LINE('',#10633,#2271);
#1884=LINE('',#10651,#2272);
#1885=LINE('',#10674,#2273);
#1886=LINE('',#10692,#2274);
#1887=LINE('',#10841,#2275);
#1888=LINE('',#10851,#2276);
#1889=LINE('',#10885,#2277);
#1890=LINE('',#10916,#2278);
#1891=LINE('',#10920,#2279);
#1892=LINE('',#10924,#2280);
#1893=LINE('',#10928,#2281);
#1894=LINE('',#10932,#2282);
#1895=LINE('',#10936,#2283);
#1896=LINE('',#10940,#2284);
#1897=LINE('',#10944,#2285);
#1898=LINE('',#11163,#2286);
#1899=LINE('',#11181,#2287);
#1900=LINE('',#11248,#2288);
#1901=LINE('',#11266,#2289);
#1902=LINE('',#11289,#2290);
#1903=LINE('',#11307,#2291);
#1904=LINE('',#11330,#2292);
#1905=LINE('',#11348,#2293);
#1906=LINE('',#11496,#2294);
#1907=LINE('',#11504,#2295);
#1908=LINE('',#11507,#2296);
#1909=LINE('',#11511,#2297);
#1910=LINE('',#11512,#2298);
#1911=LINE('',#11513,#2299);
#1912=LINE('',#11517,#2300);
#1913=LINE('',#11520,#2301);
#1914=LINE('',#11521,#2302);
#1915=LINE('',#11530,#2303);
#1916=LINE('',#11533,#2304);
#1917=LINE('',#11537,#2305);
#1918=LINE('',#11538,#2306);
#1919=LINE('',#11539,#2307);
#1920=LINE('',#11543,#2308);
#1921=LINE('',#11546,#2309);
#1922=LINE('',#11547,#2310);
#1923=LINE('',#11556,#2311);
#1924=LINE('',#11559,#2312);
#1925=LINE('',#11563,#2313);
#1926=LINE('',#11564,#2314);
#1927=LINE('',#11565,#2315);
#1928=LINE('',#11569,#2316);
#1929=LINE('',#11572,#2317);
#1930=LINE('',#11573,#2318);
#1931=LINE('',#11580,#2319);
#1932=LINE('',#11584,#2320);
#1933=LINE('',#11589,#2321);
#1934=LINE('',#11593,#2322);
#1935=LINE('',#11598,#2323);
#1936=LINE('',#11602,#2324);
#1937=LINE('',#11606,#2325);
#1938=LINE('',#11608,#2326);
#1939=LINE('',#11609,#2327);
#1940=LINE('',#11611,#2328);
#1941=LINE('',#11613,#2329);
#1942=LINE('',#11614,#2330);
#1943=LINE('',#11616,#2331);
#1944=LINE('',#11618,#2332);
#1945=LINE('',#11619,#2333);
#1946=LINE('',#11625,#2334);
#1947=LINE('',#11629,#2335);
#1948=LINE('',#11634,#2336);
#1949=LINE('',#11638,#2337);
#1950=LINE('',#11643,#2338);
#1951=LINE('',#11647,#2339);
#1952=LINE('',#11651,#2340);
#1953=LINE('',#11653,#2341);
#1954=LINE('',#11654,#2342);
#1955=LINE('',#11656,#2343);
#1956=LINE('',#11658,#2344);
#1957=LINE('',#11659,#2345);
#1958=LINE('',#11661,#2346);
#1959=LINE('',#11663,#2347);
#1960=LINE('',#11664,#2348);
#1961=LINE('',#11670,#2349);
#1962=LINE('',#11674,#2350);
#1963=LINE('',#11679,#2351);
#1964=LINE('',#11683,#2352);
#1965=LINE('',#11688,#2353);
#1966=LINE('',#11692,#2354);
#1967=LINE('',#11696,#2355);
#1968=LINE('',#11698,#2356);
#1969=LINE('',#11699,#2357);
#1970=LINE('',#11701,#2358);
#1971=LINE('',#11703,#2359);
#1972=LINE('',#11704,#2360);
#1973=LINE('',#11706,#2361);
#1974=LINE('',#11708,#2362);
#1975=LINE('',#11709,#2363);
#1976=LINE('',#11716,#2364);
#1977=LINE('',#11748,#2365);
#1978=LINE('',#11896,#2366);
#1979=LINE('',#11901,#2367);
#1980=LINE('',#11906,#2368);
#1981=LINE('',#11908,#2369);
#1982=LINE('',#11909,#2370);
#1983=LINE('',#11911,#2371);
#1984=LINE('',#11913,#2372);
#1985=LINE('',#11914,#2373);
#1986=LINE('',#11916,#2374);
#1987=LINE('',#11918,#2375);
#1988=LINE('',#11919,#2376);
#1989=LINE('',#11925,#2377);
#1990=LINE('',#11973,#2378);
#1991=LINE('',#11989,#2379);
#1992=LINE('',#11993,#2380);
#1993=LINE('',#11997,#2381);
#1994=LINE('',#12002,#2382);
#1995=LINE('',#12004,#2383);
#1996=LINE('',#12006,#2384);
#1997=LINE('',#12007,#2385);
#1998=LINE('',#12009,#2386);
#1999=LINE('',#12011,#2387);
#2000=LINE('',#12012,#2388);
#2001=LINE('',#12014,#2389);
#2002=LINE('',#12015,#2390);
#2003=LINE('',#12021,#2391);
#2004=LINE('',#12026,#2392);
#2005=LINE('',#12028,#2393);
#2006=LINE('',#12030,#2394);
#2007=LINE('',#12031,#2395);
#2008=LINE('',#12033,#2396);
#2009=LINE('',#12035,#2397);
#2010=LINE('',#12036,#2398);
#2011=LINE('',#12038,#2399);
#2012=LINE('',#12039,#2400);
#2013=LINE('',#12045,#2401);
#2014=LINE('',#12101,#2402);
#2015=LINE('',#12157,#2403);
#2016=LINE('',#12159,#2404);
#2017=LINE('',#12161,#2405);
#2018=LINE('',#12166,#2406);
#2019=LINE('',#12167,#2407);
#2020=LINE('',#12169,#2408);
#2021=LINE('',#12171,#2409);
#2022=LINE('',#12174,#2410);
#2023=LINE('',#12176,#2411);
#2024=LINE('',#12179,#2412);
#2025=LINE('',#12181,#2413);
#2026=LINE('',#12184,#2414);
#2027=LINE('',#12186,#2415);
#2028=LINE('',#12189,#2416);
#2029=LINE('',#12191,#2417);
#2030=LINE('',#12194,#2418);
#2031=LINE('',#12196,#2419);
#2032=LINE('',#12199,#2420);
#2033=LINE('',#12201,#2421);
#2034=LINE('',#12204,#2422);
#2035=LINE('',#12206,#2423);
#2036=LINE('',#12209,#2424);
#2037=LINE('',#12211,#2425);
#2038=LINE('',#12218,#2426);
#2039=LINE('',#12230,#2427);
#2040=LINE('',#12233,#2428);
#2041=LINE('',#12238,#2429);
#2042=LINE('',#12244,#2430);
#2043=LINE('',#12256,#2431);
#2044=LINE('',#12259,#2432);
#2045=LINE('',#12264,#2433);
#2046=LINE('',#12270,#2434);
#2047=LINE('',#12282,#2435);
#2048=LINE('',#12285,#2436);
#2049=LINE('',#12290,#2437);
#2050=LINE('',#12296,#2438);
#2051=LINE('',#12308,#2439);
#2052=LINE('',#12311,#2440);
#2053=LINE('',#12316,#2441);
#2054=LINE('',#12321,#2442);
#2055=LINE('',#12325,#2443);
#2056=LINE('',#12330,#2444);
#2057=LINE('',#12334,#2445);
#2058=LINE('',#12341,#2446);
#2059=LINE('',#12344,#2447);
#2060=LINE('',#12348,#2448);
#2061=LINE('',#12374,#2449);
#2062=LINE('',#12400,#2450);
#2063=LINE('',#12425,#2451);
#2064=LINE('',#12446,#2452);
#2065=LINE('',#12471,#2453);
#2066=LINE('',#12492,#2454);
#2067=LINE('',#12516,#2455);
#2068=LINE('',#12548,#2456);
#2069=LINE('',#12551,#2457);
#2070=LINE('',#12555,#2458);
#2071=LINE('',#12581,#2459);
#2072=LINE('',#12607,#2460);
#2073=LINE('',#12632,#2461);
#2074=LINE('',#12653,#2462);
#2075=LINE('',#12678,#2463);
#2076=LINE('',#12699,#2464);
#2077=LINE('',#12723,#2465);
#2078=LINE('',#12753,#2466);
#2079=LINE('',#12779,#2467);
#2080=LINE('',#12805,#2468);
#2081=LINE('',#12830,#2469);
#2082=LINE('',#12851,#2470);
#2083=LINE('',#12876,#2471);
#2084=LINE('',#12897,#2472);
#2085=LINE('',#12921,#2473);
#2086=LINE('',#12953,#2474);
#2087=LINE('',#12956,#2475);
#2088=LINE('',#12960,#2476);
#2089=LINE('',#12964,#2477);
#2090=LINE('',#12970,#2478);
#2091=LINE('',#12973,#2479);
#2092=LINE('',#12975,#2480);
#2093=LINE('',#12978,#2481);
#2094=LINE('',#12980,#2482);
#2095=LINE('',#12983,#2483);
#2096=LINE('',#12988,#2484);
#2097=LINE('',#12990,#2485);
#2098=LINE('',#12991,#2486);
#2099=LINE('',#12993,#2487);
#2100=LINE('',#12995,#2488);
#2101=LINE('',#12996,#2489);
#2102=LINE('',#12998,#2490);
#2103=LINE('',#13000,#2491);
#2104=LINE('',#13001,#2492);
#2105=LINE('',#13003,#2493);
#2106=LINE('',#13006,#2494);
#2107=LINE('',#13008,#2495);
#2108=LINE('',#13009,#2496);
#2109=LINE('',#13011,#2497);
#2110=LINE('',#13013,#2498);
#2111=LINE('',#13014,#2499);
#2112=LINE('',#13016,#2500);
#2113=LINE('',#13018,#2501);
#2114=LINE('',#13019,#2502);
#2115=LINE('',#13024,#2503);
#2116=LINE('',#13027,#2504);
#2117=LINE('',#13029,#2505);
#2118=LINE('',#13032,#2506);
#2119=LINE('',#13034,#2507);
#2120=LINE('',#13037,#2508);
#2121=LINE('',#13044,#2509);
#2122=LINE('',#13046,#2510);
#2123=LINE('',#13066,#2511);
#2124=LINE('',#13073,#2512);
#2125=LINE('',#13080,#2513);
#2126=LINE('',#13087,#2514);
#2127=LINE('',#13094,#2515);
#2128=LINE('',#13101,#2516);
#2129=LINE('',#13108,#2517);
#2130=LINE('',#13112,#2518);
#2131=LINE('',#13648,#2519);
#2132=LINE('',#13650,#2520);
#2133=LINE('',#13652,#2521);
#2134=LINE('',#13654,#2522);
#2135=LINE('',#13656,#2523);
#2136=LINE('',#13663,#2524);
#2137=LINE('',#13665,#2525);
#2138=LINE('',#13685,#2526);
#2139=LINE('',#13692,#2527);
#2140=LINE('',#13694,#2528);
#2141=LINE('',#13714,#2529);
#2142=LINE('',#13721,#2530);
#2143=LINE('',#13728,#2531);
#2144=LINE('',#13735,#2532);
#2145=LINE('',#13742,#2533);
#2146=LINE('',#13749,#2534);
#2147=LINE('',#13756,#2535);
#2148=LINE('',#13759,#2536);
#2149=LINE('',#13763,#2537);
#2150=LINE('',#13767,#2538);
#2151=LINE('',#13771,#2539);
#2152=LINE('',#13775,#2540);
#2153=LINE('',#13779,#2541);
#2154=LINE('',#13783,#2542);
#2155=LINE('',#13787,#2543);
#2156=LINE('',#13793,#2544);
#2157=LINE('',#13798,#2545);
#2158=LINE('',#13803,#2546);
#2159=LINE('',#13808,#2547);
#2160=LINE('',#13813,#2548);
#2161=LINE('',#13818,#2549);
#2162=LINE('',#13823,#2550);
#2163=LINE('',#13828,#2551);
#2164=LINE('',#13830,#2552);
#2165=LINE('',#13832,#2553);
#2166=LINE('',#13835,#2554);
#2167=LINE('',#13836,#2555);
#2168=LINE('',#13839,#2556);
#2169=LINE('',#13840,#2557);
#2170=LINE('',#13893,#2558);
#2171=LINE('',#13895,#2559);
#2172=LINE('',#13898,#2560);
#2173=LINE('',#13899,#2561);
#2174=LINE('',#13902,#2562);
#2175=LINE('',#13903,#2563);
#2176=LINE('',#13956,#2564);
#2177=LINE('',#13958,#2565);
#2178=LINE('',#13961,#2566);
#2179=LINE('',#13962,#2567);
#2180=LINE('',#13965,#2568);
#2181=LINE('',#13966,#2569);
#2182=LINE('',#14019,#2570);
#2183=LINE('',#14021,#2571);
#2184=LINE('',#14024,#2572);
#2185=LINE('',#14026,#2573);
#2186=LINE('',#14029,#2574);
#2187=LINE('',#14031,#2575);
#2188=LINE('',#14078,#2576);
#2189=LINE('',#14088,#2577);
#2190=LINE('',#14094,#2578);
#2191=VECTOR('',#6913,60.0123183146203);
#2192=VECTOR('',#6914,74.);
#2193=VECTOR('',#6915,60.0123183146203);
#2194=VECTOR('',#6916,10.);
#2195=VECTOR('',#6917,20.1794558564032);
#2196=VECTOR('',#6920,20.1794558568838);
#2197=VECTOR('',#6921,10.);
#2198=VECTOR('',#6946,74.);
#2199=VECTOR('',#6947,45.6680057154832);
#2200=VECTOR('',#6948,74.);
#2201=VECTOR('',#6949,45.6680057154831);
#2202=VECTOR('',#6962,45.6680057154832);
#2203=VECTOR('',#6963,74.);
#2204=VECTOR('',#6964,45.6680057154831);
#2205=VECTOR('',#6965,74.);
#2206=VECTOR('',#6970,14.);
#2207=VECTOR('',#6977,13.897506768291);
#2208=VECTOR('',#6980,37.);
#2209=VECTOR('',#6981,37.);
#2210=VECTOR('',#6984,10.);
#2211=VECTOR('',#6985,10.);
#2212=VECTOR('',#6990,74.);
#2213=VECTOR('',#6991,60.0123511269393);
#2214=VECTOR('',#6992,10.);
#2215=VECTOR('',#6993,20.1794558568839);
#2216=VECTOR('',#6996,20.1794558564032);
#2217=VECTOR('',#6997,10.);
#2218=VECTOR('',#6998,60.0123511269481);
#2219=VECTOR('',#7009,77.1122755947453);
#2220=VECTOR('',#7010,10.);
#2221=VECTOR('',#7013,10.);
#2222=VECTOR('',#7014,77.1122755947453);
#2223=VECTOR('',#7019,10.);
#2224=VECTOR('',#7020,77.1122755947453);
#2225=VECTOR('',#7023,77.1122755947453);
#2226=VECTOR('',#7024,10.);
#2227=VECTOR('',#7027,4.99999999999998);
#2228=VECTOR('',#7030,4.99999999999998);
#2229=VECTOR('',#7033,5.);
#2230=VECTOR('',#7034,5.);
#2231=VECTOR('',#7037,5.);
#2232=VECTOR('',#7038,5.);
#2233=VECTOR('',#7041,10.);
#2234=VECTOR('',#7042,10.);
#2235=VECTOR('',#7043,10.);
#2236=VECTOR('',#7046,37.);
#2237=VECTOR('',#7047,37.);
#2238=VECTOR('',#7048,10.);
#2239=VECTOR('',#7051,5.);
#2240=VECTOR('',#7054,5.);
#2241=VECTOR('',#7057,5.00000000000002);
#2242=VECTOR('',#7060,5.00000000000002);
#2243=VECTOR('',#7063,5.);
#2244=VECTOR('',#7066,5.);
#2245=VECTOR('',#7069,10.);
#2246=VECTOR('',#7070,10.);
#2247=VECTOR('',#7085,17.5);
#2248=VECTOR('',#7094,17.5);
#2249=VECTOR('',#7101,13.897506768291);
#2250=VECTOR('',#7108,20.);
#2251=VECTOR('',#7117,3.99999999999999);
#2252=VECTOR('',#7120,15.9631510575949);
#2253=VECTOR('',#7123,3.99999999999999);
#2254=VECTOR('',#7126,3.99999999999999);
#2255=VECTOR('',#7129,15.9631510575949);
#2256=VECTOR('',#7132,3.99999999999999);
#2257=VECTOR('',#7141,20.5);
#2258=VECTOR('',#7142,20.5);
#2259=VECTOR('',#7147,12.);
#2260=VECTOR('',#7150,12.);
#2261=VECTOR('',#7153,12.);
#2262=VECTOR('',#7156,12.);
#2263=VECTOR('',#7159,12.);
#2264=VECTOR('',#7162,12.);
#2265=VECTOR('',#7165,12.);
#2266=VECTOR('',#7168,12.);
#2267=VECTOR('',#7185,10.0757988598381);
#2268=VECTOR('',#7188,10.0757988598381);
#2269=VECTOR('',#7209,10.0757988598381);
#2270=VECTOR('',#7212,10.0757988598381);
#2271=VECTOR('',#7225,10.0757988598381);
#2272=VECTOR('',#7228,10.0757988598381);
#2273=VECTOR('',#7241,10.0757988598381);
#2274=VECTOR('',#7244,10.0757988598381);
#2275=VECTOR('',#7287,17.5);
#2276=VECTOR('',#7300,20.5);
#2277=VECTOR('',#7301,20.5);
#2278=VECTOR('',#7306,12.);
#2279=VECTOR('',#7309,12.);
#2280=VECTOR('',#7312,12.);
#2281=VECTOR('',#7315,12.);
#2282=VECTOR('',#7318,12.);
#2283=VECTOR('',#7321,12.);
#2284=VECTOR('',#7324,12.);
#2285=VECTOR('',#7327,12.);
#2286=VECTOR('',#7346,10.0757988598381);
#2287=VECTOR('',#7349,10.0757988598381);
#2288=VECTOR('',#7370,10.0757988598381);
#2289=VECTOR('',#7373,10.0757988598381);
#2290=VECTOR('',#7386,10.0757988598381);
#2291=VECTOR('',#7389,10.0757988598381);
#2292=VECTOR('',#7402,10.0757988598381);
#2293=VECTOR('',#7405,10.0757988598381);
#2294=VECTOR('',#7448,17.5);
#2295=VECTOR('',#7457,2.00000000000281);
#2296=VECTOR('',#7460,2.00000000000281);
#2297=VECTOR('',#7463,1.99999999999748);
#2298=VECTOR('',#7464,55.9999999999999);
#2299=VECTOR('',#7465,55.9999999999999);
#2300=VECTOR('',#7470,56.0000000000002);
#2301=VECTOR('',#7473,2.0000000000017);
#2302=VECTOR('',#7474,56.0000000000002);
#2303=VECTOR('',#7485,2.0000000000028);
#2304=VECTOR('',#7488,2.00000000000279);
#2305=VECTOR('',#7491,2.00000000000043);
#2306=VECTOR('',#7492,56.);
#2307=VECTOR('',#7493,56.);
#2308=VECTOR('',#7498,56.);
#2309=VECTOR('',#7501,2.0000000000028);
#2310=VECTOR('',#7502,56.);
#2311=VECTOR('',#7513,2.0000000000028);
#2312=VECTOR('',#7516,2.00000000000278);
#2313=VECTOR('',#7519,1.99999999999811);
#2314=VECTOR('',#7520,55.9999999999998);
#2315=VECTOR('',#7521,55.9999999999998);
#2316=VECTOR('',#7526,56.0000000000001);
#2317=VECTOR('',#7529,2.00000000000235);
#2318=VECTOR('',#7530,56.0000000000001);
#2319=VECTOR('',#7539,4.);
#2320=VECTOR('',#7542,4.);
#2321=VECTOR('',#7547,4.);
#2322=VECTOR('',#7550,3.99999999999998);
#2323=VECTOR('',#7555,4.);
#2324=VECTOR('',#7558,3.99999999999998);
#2325=VECTOR('',#7563,1.04078523274219);
#2326=VECTOR('',#7564,1.0000000000001);
#2327=VECTOR('',#7565,1.04078523274216);
#2328=VECTOR('',#7566,1.04078523274217);
#2329=VECTOR('',#7567,0.999999999999985);
#2330=VECTOR('',#7568,1.04078523274216);
#2331=VECTOR('',#7569,1.04078523274218);
#2332=VECTOR('',#7570,1.);
#2333=VECTOR('',#7571,1.04078523274217);
#2334=VECTOR('',#7576,4.00000000000002);
#2335=VECTOR('',#7579,3.99999999999999);
#2336=VECTOR('',#7584,4.);
#2337=VECTOR('',#7587,4.00000000000005);
#2338=VECTOR('',#7592,4.00000000000001);
#2339=VECTOR('',#7595,4.);
#2340=VECTOR('',#7600,1.04078523274219);
#2341=VECTOR('',#7601,1.0000000000001);
#2342=VECTOR('',#7602,1.04078523274216);
#2343=VECTOR('',#7603,1.04078523274223);
#2344=VECTOR('',#7604,0.99999999999995);
#2345=VECTOR('',#7605,1.04078523274216);
#2346=VECTOR('',#7606,1.04078523274216);
#2347=VECTOR('',#7607,1.00000000000002);
#2348=VECTOR('',#7608,1.04078523274214);
#2349=VECTOR('',#7613,4.);
#2350=VECTOR('',#7616,4.);
#2351=VECTOR('',#7621,4.);
#2352=VECTOR('',#7624,4.);
#2353=VECTOR('',#7629,4.);
#2354=VECTOR('',#7632,4.);
#2355=VECTOR('',#7637,1.0407852327422);
#2356=VECTOR('',#7638,1.00000000000002);
#2357=VECTOR('',#7639,1.04078523274213);
#2358=VECTOR('',#7640,1.04078523274222);
#2359=VECTOR('',#7641,1.00000000000002);
#2360=VECTOR('',#7642,1.04078523274215);
#2361=VECTOR('',#7643,1.0407852327422);
#2362=VECTOR('',#7644,0.999999999999994);
#2363=VECTOR('',#7645,1.04078523274217);
#2364=VECTOR('',#7652,28.1634258170599);
#2365=VECTOR('',#7653,28.1634258170599);
#2366=VECTOR('',#7668,23.1634258170599);
#2367=VECTOR('',#7675,15.);
#2368=VECTOR('',#7680,1.04078523274216);
#2369=VECTOR('',#7681,1.);
#2370=VECTOR('',#7682,1.0407852327422);
#2371=VECTOR('',#7683,1.0407852327422);
#2372=VECTOR('',#7684,1.);
#2373=VECTOR('',#7685,1.0407852327422);
#2374=VECTOR('',#7686,1.04078523274218);
#2375=VECTOR('',#7687,1.);
#2376=VECTOR('',#7688,1.04078523274223);
#2377=VECTOR('',#7695,17.);
#2378=VECTOR('',#7698,13.);
#2379=VECTOR('',#7701,17.);
#2380=VECTOR('',#7706,15.);
#2381=VECTOR('',#7711,15.);
#2382=VECTOR('',#7716,1.0407852327422);
#2383=VECTOR('',#7717,1.04078523274217);
#2384=VECTOR('',#7718,1.);
#2385=VECTOR('',#7719,1.0407852327422);
#2386=VECTOR('',#7720,1.04078523274218);
#2387=VECTOR('',#7721,1.);
#2388=VECTOR('',#7722,1.0407852327422);
#2389=VECTOR('',#7723,1.0407852327422);
#2390=VECTOR('',#7724,1.00000000000001);
#2391=VECTOR('',#7731,17.);
#2392=VECTOR('',#7736,1.0407852327422);
#2393=VECTOR('',#7737,1.04078523274218);
#2394=VECTOR('',#7738,1.00000000000002);
#2395=VECTOR('',#7739,1.04078523274219);
#2396=VECTOR('',#7740,1.0407852327422);
#2397=VECTOR('',#7741,1.);
#2398=VECTOR('',#7742,1.04078523274225);
#2399=VECTOR('',#7743,1.0407852327422);
#2400=VECTOR('',#7744,1.00000000000001);
#2401=VECTOR('',#7751,17.);
#2402=VECTOR('',#7754,13.);
#2403=VECTOR('',#7757,13.);
#2404=VECTOR('',#7760,17.);
#2405=VECTOR('',#7763,17.);
#2406=VECTOR('',#7770,20.);
#2407=VECTOR('',#7771,20.);
#2408=VECTOR('',#7774,4.);
#2409=VECTOR('',#7777,4.);
#2410=VECTOR('',#7782,4.);
#2411=VECTOR('',#7785,4.);
#2412=VECTOR('',#7790,4.);
#2413=VECTOR('',#7793,4.);
#2414=VECTOR('',#7798,4.);
#2415=VECTOR('',#7801,4.);
#2416=VECTOR('',#7806,4.00000000000005);
#2417=VECTOR('',#7809,4.00000000000003);
#2418=VECTOR('',#7814,4.00000000000002);
#2419=VECTOR('',#7817,4.);
#2420=VECTOR('',#7822,4.);
#2421=VECTOR('',#7825,4.);
#2422=VECTOR('',#7830,4.);
#2423=VECTOR('',#7833,4.);
#2424=VECTOR('',#7838,3.99999999999998);
#2425=VECTOR('',#7841,3.99999999999998);
#2426=VECTOR('',#7850,3.99999999999999);
#2427=VECTOR('',#7865,0.899999999999994);
#2428=VECTOR('',#7870,1.8);
#2429=VECTOR('',#7877,3.49999999999999);
#2430=VECTOR('',#7884,4.00000000000001);
#2431=VECTOR('',#7899,0.899999999999993);
#2432=VECTOR('',#7904,1.8);
#2433=VECTOR('',#7911,3.50000000000002);
#2434=VECTOR('',#7918,4.);
#2435=VECTOR('',#7933,0.899999999999989);
#2436=VECTOR('',#7938,1.80000000000001);
#2437=VECTOR('',#7945,3.49999999999992);
#2438=VECTOR('',#7952,4.00000000000013);
#2439=VECTOR('',#7967,0.899999999999984);
#2440=VECTOR('',#7972,1.8);
#2441=VECTOR('',#7979,3.50000000000012);
#2442=VECTOR('',#7984,3.99999999999999);
#2443=VECTOR('',#7987,3.99999999999998);
#2444=VECTOR('',#7992,3.99999999999999);
#2445=VECTOR('',#7995,3.99999999999996);
#2446=VECTOR('',#8002,57.);
#2447=VECTOR('',#8005,57.);
#2448=VECTOR('',#8008,13.3544586520373);
#2449=VECTOR('',#8009,13.3544586520371);
#2450=VECTOR('',#8012,13.3319433271509);
#2451=VECTOR('',#8013,13.3319433271509);
#2452=VECTOR('',#8016,13.2704303156128);
#2453=VECTOR('',#8017,13.2704303156126);
#2454=VECTOR('',#8020,3.88631345570718);
#2455=VECTOR('',#8021,3.88631345570666);
#2456=VECTOR('',#8026,57.);
#2457=VECTOR('',#8029,57.);
#2458=VECTOR('',#8032,13.3544586520373);
#2459=VECTOR('',#8033,13.3544586520371);
#2460=VECTOR('',#8036,13.3319433271511);
#2461=VECTOR('',#8037,13.3319433271509);
#2462=VECTOR('',#8040,13.2704303156128);
#2463=VECTOR('',#8041,13.2704303156126);
#2464=VECTOR('',#8044,3.88631345570709);
#2465=VECTOR('',#8045,3.88631345570659);
#2466=VECTOR('',#8048,13.3544586520373);
#2467=VECTOR('',#8049,13.3544586520371);
#2468=VECTOR('',#8052,13.331943327151);
#2469=VECTOR('',#8053,13.3319433271509);
#2470=VECTOR('',#8056,13.2704303156128);
#2471=VECTOR('',#8057,13.2704303156126);
#2472=VECTOR('',#8060,3.88631345570711);
#2473=VECTOR('',#8061,3.8863134557066);
#2474=VECTOR('',#8066,57.);
#2475=VECTOR('',#8069,57.);
#2476=VECTOR('',#8072,3.99999999999998);
#2477=VECTOR('',#8075,3.99999999999998);
#2478=VECTOR('',#8082,0.561081020730737);
#2479=VECTOR('',#8085,0.561081020730727);
#2480=VECTOR('',#8086,0.561081020730758);
#2481=VECTOR('',#8089,0.561081020730749);
#2482=VECTOR('',#8090,0.561081020730754);
#2483=VECTOR('',#8093,0.561081020730736);
#2484=VECTOR('',#8098,0.999999999999974);
#2485=VECTOR('',#8099,1.00000000000001);
#2486=VECTOR('',#8100,0.999999999999884);
#2487=VECTOR('',#8101,1.);
#2488=VECTOR('',#8102,1.00000000000001);
#2489=VECTOR('',#8103,0.999999999999921);
#2490=VECTOR('',#8104,0.999999999999996);
#2491=VECTOR('',#8105,0.999999999999991);
#2492=VECTOR('',#8106,0.99999999999989);
#2493=VECTOR('',#8109,17.);
#2494=VECTOR('',#8112,0.999999999999894);
#2495=VECTOR('',#8113,1.00000000000001);
#2496=VECTOR('',#8114,0.999999999999984);
#2497=VECTOR('',#8115,0.99999999999989);
#2498=VECTOR('',#8116,0.999999999999991);
#2499=VECTOR('',#8117,0.999999999999996);
#2500=VECTOR('',#8118,0.999999999999925);
#2501=VECTOR('',#8119,1.00000000000001);
#2502=VECTOR('',#8120,1.00000000000002);
#2503=VECTOR('',#8125,0.56108102073074);
#2504=VECTOR('',#8128,0.561081020730741);
#2505=VECTOR('',#8129,0.561081020730736);
#2506=VECTOR('',#8132,0.561081020730754);
#2507=VECTOR('',#8133,0.561081020730749);
#2508=VECTOR('',#8136,0.561081020730719);
#2509=VECTOR('',#8145,4.00000000000012);
#2510=VECTOR('',#8146,0.519472430034522);
#2511=VECTOR('',#8147,0.519472430034611);
#2512=VECTOR('',#8156,4.00000000000001);
#2513=VECTOR('',#8165,4.00000000000001);
#2514=VECTOR('',#8174,4.);
#2515=VECTOR('',#8183,3.50000000000012);
#2516=VECTOR('',#8192,3.5);
#2517=VECTOR('',#8201,3.49999999999992);
#2518=VECTOR('',#8206,12.9999999999984);
#2519=VECTOR('',#8217,3.49999999999998);
#2520=VECTOR('',#8220,2.80000000000012);
#2521=VECTOR('',#8223,2.79999999999998);
#2522=VECTOR('',#8226,2.79999999999991);
#2523=VECTOR('',#8229,2.79999999999999);
#2524=VECTOR('',#8238,4.00000000000012);
#2525=VECTOR('',#8239,0.519472430034534);
#2526=VECTOR('',#8240,0.519472430034598);
#2527=VECTOR('',#8249,4.00000000000012);
#2528=VECTOR('',#8250,0.519472430034482);
#2529=VECTOR('',#8251,0.519472430034555);
#2530=VECTOR('',#8260,4.00000000000001);
#2531=VECTOR('',#8269,4.00000000000001);
#2532=VECTOR('',#8278,4.00000000000001);
#2533=VECTOR('',#8287,4.00000000000001);
#2534=VECTOR('',#8296,4.);
#2535=VECTOR('',#8305,4.);
#2536=VECTOR('',#8308,2.80000000000012);
#2537=VECTOR('',#8313,2.80000000000012);
#2538=VECTOR('',#8318,2.79999999999998);
#2539=VECTOR('',#8323,2.79999999999998);
#2540=VECTOR('',#8328,2.79999999999991);
#2541=VECTOR('',#8333,2.79999999999991);
#2542=VECTOR('',#8338,2.79999999999999);
#2543=VECTOR('',#8343,2.79999999999999);
#2544=VECTOR('',#8352,3.50000000000012);
#2545=VECTOR('',#8359,3.50000000000012);
#2546=VECTOR('',#8366,3.5);
#2547=VECTOR('',#8373,3.5);
#2548=VECTOR('',#8380,3.49999999999992);
#2549=VECTOR('',#8387,3.49999999999992);
#2550=VECTOR('',#8394,3.49999999999998);
#2551=VECTOR('',#8401,3.49999999999998);
#2552=VECTOR('',#8404,57.);
#2553=VECTOR('',#8407,57.);
#2554=VECTOR('',#8410,0.519472430034682);
#2555=VECTOR('',#8411,43.8431457505075);
#2556=VECTOR('',#8414,43.8431457505077);
#2557=VECTOR('',#8415,0.519472430034611);
#2558=VECTOR('',#8420,57.);
#2559=VECTOR('',#8423,57.);
#2560=VECTOR('',#8426,0.51947243003468);
#2561=VECTOR('',#8427,43.8431457505077);
#2562=VECTOR('',#8430,43.8431457505077);
#2563=VECTOR('',#8431,0.519472430034606);
#2564=VECTOR('',#8436,57.);
#2565=VECTOR('',#8439,57.);
#2566=VECTOR('',#8442,0.5194724300347);
#2567=VECTOR('',#8443,43.8431457505077);
#2568=VECTOR('',#8446,43.8431457505077);
#2569=VECTOR('',#8447,0.519472430034622);
#2570=VECTOR('',#8452,3.99999999999998);
#2571=VECTOR('',#8455,3.99999999999998);
#2572=VECTOR('',#8460,3.99999999999997);
#2573=VECTOR('',#8463,4.);
#2574=VECTOR('',#8468,3.99999999999998);
#2575=VECTOR('',#8471,3.99999999999998);
#2576=VECTOR('',#8560,16.);
#2577=VECTOR('',#8573,14.);
#2578=VECTOR('',#8582,12.);
#2579=VERTEX_POINT('',#8596);
#2580=VERTEX_POINT('',#8597);
#2581=VERTEX_POINT('',#8599);
#2582=VERTEX_POINT('',#8601);
#2583=VERTEX_POINT('',#8603);
#2584=VERTEX_POINT('',#8605);
#2585=VERTEX_POINT('',#8607);
#2586=VERTEX_POINT('',#8609);
#2587=VERTEX_POINT('',#8612);
#2588=VERTEX_POINT('',#8614);
#2589=VERTEX_POINT('',#8616);
#2590=VERTEX_POINT('',#8619);
#2591=VERTEX_POINT('',#8620);
#2592=VERTEX_POINT('',#8622);
#2593=VERTEX_POINT('',#8624);
#2594=VERTEX_POINT('',#8626);
#2595=VERTEX_POINT('',#8628);
#2596=VERTEX_POINT('',#8630);
#2597=VERTEX_POINT('',#8632);
#2598=VERTEX_POINT('',#8635);
#2599=VERTEX_POINT('',#8636);
#2600=VERTEX_POINT('',#8638);
#2601=VERTEX_POINT('',#8640);
#2602=VERTEX_POINT('',#8643);
#2603=VERTEX_POINT('',#8645);
#2604=VERTEX_POINT('',#8647);
#2605=VERTEX_POINT('',#8649);
#2606=VERTEX_POINT('',#8651);
#2607=VERTEX_POINT('',#8653);
#2608=VERTEX_POINT('',#8655);
#2609=VERTEX_POINT('',#8656);
#2610=VERTEX_POINT('',#8658);
#2611=VERTEX_POINT('',#8660);
#2612=VERTEX_POINT('',#8664);
#2613=VERTEX_POINT('',#8666);
#2614=VERTEX_POINT('',#8669);
#2615=VERTEX_POINT('',#8670);
#2616=VERTEX_POINT('',#8747);
#2617=VERTEX_POINT('',#8748);
#2618=VERTEX_POINT('',#8826);
#2619=VERTEX_POINT('',#8830);
#2620=VERTEX_POINT('',#8831);
#2621=VERTEX_POINT('',#8833);
#2622=VERTEX_POINT('',#8852);
#2623=VERTEX_POINT('',#8871);
#2624=VERTEX_POINT('',#8873);
#2625=VERTEX_POINT('',#8875);
#2626=VERTEX_POINT('',#8877);
#2627=VERTEX_POINT('',#8903);
#2628=VERTEX_POINT('',#8907);
#2629=VERTEX_POINT('',#8908);
#2630=VERTEX_POINT('',#8910);
#2631=VERTEX_POINT('',#8912);
#2632=VERTEX_POINT('',#8914);
#2633=VERTEX_POINT('',#8916);
#2634=VERTEX_POINT('',#8918);
#2635=VERTEX_POINT('',#8920);
#2636=VERTEX_POINT('',#8923);
#2637=VERTEX_POINT('',#8925);
#2638=VERTEX_POINT('',#8927);
#2639=VERTEX_POINT('',#8930);
#2640=VERTEX_POINT('',#8931);
#2641=VERTEX_POINT('',#9121);
#2642=VERTEX_POINT('',#9123);
#2643=VERTEX_POINT('',#9321);
#2644=VERTEX_POINT('',#9328);
#2645=VERTEX_POINT('',#9337);
#2646=VERTEX_POINT('',#9338);
#2647=VERTEX_POINT('',#9388);
#2648=VERTEX_POINT('',#9389);
#2649=VERTEX_POINT('',#9548);
#2650=VERTEX_POINT('',#9624);
#2651=VERTEX_POINT('',#9787);
#2652=VERTEX_POINT('',#9836);
#2653=VERTEX_POINT('',#10149);
#2654=VERTEX_POINT('',#10153);
#2655=VERTEX_POINT('',#10157);
#2656=VERTEX_POINT('',#10161);
#2657=VERTEX_POINT('',#10164);
#2658=VERTEX_POINT('',#10171);
#2659=VERTEX_POINT('',#10192);
#2660=VERTEX_POINT('',#10193);
#2661=VERTEX_POINT('',#10196);
#2662=VERTEX_POINT('',#10198);
#2663=VERTEX_POINT('',#10207);
#2664=VERTEX_POINT('',#10230);
#2665=VERTEX_POINT('',#10232);
#2666=VERTEX_POINT('',#10260);
#2667=VERTEX_POINT('',#10261);
#2668=VERTEX_POINT('',#10263);
#2669=VERTEX_POINT('',#10265);
#2670=VERTEX_POINT('',#10268);
#2671=VERTEX_POINT('',#10269);
#2672=VERTEX_POINT('',#10271);
#2673=VERTEX_POINT('',#10273);
#2674=VERTEX_POINT('',#10276);
#2675=VERTEX_POINT('',#10277);
#2676=VERTEX_POINT('',#10279);
#2677=VERTEX_POINT('',#10281);
#2678=VERTEX_POINT('',#10284);
#2679=VERTEX_POINT('',#10285);
#2680=VERTEX_POINT('',#10287);
#2681=VERTEX_POINT('',#10289);
#2682=VERTEX_POINT('',#10292);
#2683=VERTEX_POINT('',#10337);
#2684=VERTEX_POINT('',#10382);
#2685=VERTEX_POINT('',#10428);
#2686=VERTEX_POINT('',#10431);
#2687=VERTEX_POINT('',#10433);
#2688=VERTEX_POINT('',#10496);
#2689=VERTEX_POINT('',#10497);
#2690=VERTEX_POINT('',#10499);
#2691=VERTEX_POINT('',#10506);
#2692=VERTEX_POINT('',#10508);
#2693=VERTEX_POINT('',#10515);
#2694=VERTEX_POINT('',#10517);
#2695=VERTEX_POINT('',#10524);
#2696=VERTEX_POINT('',#10581);
#2697=VERTEX_POINT('',#10582);
#2698=VERTEX_POINT('',#10584);
#2699=VERTEX_POINT('',#10591);
#2700=VERTEX_POINT('',#10593);
#2701=VERTEX_POINT('',#10600);
#2702=VERTEX_POINT('',#10602);
#2703=VERTEX_POINT('',#10609);
#2704=VERTEX_POINT('',#10622);
#2705=VERTEX_POINT('',#10623);
#2706=VERTEX_POINT('',#10625);
#2707=VERTEX_POINT('',#10632);
#2708=VERTEX_POINT('',#10634);
#2709=VERTEX_POINT('',#10641);
#2710=VERTEX_POINT('',#10643);
#2711=VERTEX_POINT('',#10650);
#2712=VERTEX_POINT('',#10663);
#2713=VERTEX_POINT('',#10664);
#2714=VERTEX_POINT('',#10666);
#2715=VERTEX_POINT('',#10673);
#2716=VERTEX_POINT('',#10675);
#2717=VERTEX_POINT('',#10682);
#2718=VERTEX_POINT('',#10684);
#2719=VERTEX_POINT('',#10691);
#2720=VERTEX_POINT('',#10840);
#2721=VERTEX_POINT('',#10846);
#2722=VERTEX_POINT('',#10847);
#2723=VERTEX_POINT('',#10850);
#2724=VERTEX_POINT('',#10852);
#2725=VERTEX_POINT('',#10861);
#2726=VERTEX_POINT('',#10884);
#2727=VERTEX_POINT('',#10886);
#2728=VERTEX_POINT('',#10914);
#2729=VERTEX_POINT('',#10915);
#2730=VERTEX_POINT('',#10917);
#2731=VERTEX_POINT('',#10919);
#2732=VERTEX_POINT('',#10922);
#2733=VERTEX_POINT('',#10923);
#2734=VERTEX_POINT('',#10925);
#2735=VERTEX_POINT('',#10927);
#2736=VERTEX_POINT('',#10930);
#2737=VERTEX_POINT('',#10931);
#2738=VERTEX_POINT('',#10933);
#2739=VERTEX_POINT('',#10935);
#2740=VERTEX_POINT('',#10938);
#2741=VERTEX_POINT('',#10939);
#2742=VERTEX_POINT('',#10941);
#2743=VERTEX_POINT('',#10943);
#2744=VERTEX_POINT('',#10946);
#2745=VERTEX_POINT('',#10991);
#2746=VERTEX_POINT('',#11036);
#2747=VERTEX_POINT('',#11082);
#2748=VERTEX_POINT('',#11084);
#2749=VERTEX_POINT('',#11087);
#2750=VERTEX_POINT('',#11089);
#2751=VERTEX_POINT('',#11152);
#2752=VERTEX_POINT('',#11153);
#2753=VERTEX_POINT('',#11155);
#2754=VERTEX_POINT('',#11162);
#2755=VERTEX_POINT('',#11164);
#2756=VERTEX_POINT('',#11171);
#2757=VERTEX_POINT('',#11173);
#2758=VERTEX_POINT('',#11180);
#2759=VERTEX_POINT('',#11237);
#2760=VERTEX_POINT('',#11238);
#2761=VERTEX_POINT('',#11240);
#2762=VERTEX_POINT('',#11247);
#2763=VERTEX_POINT('',#11249);
#2764=VERTEX_POINT('',#11256);
#2765=VERTEX_POINT('',#11258);
#2766=VERTEX_POINT('',#11265);
#2767=VERTEX_POINT('',#11278);
#2768=VERTEX_POINT('',#11279);
#2769=VERTEX_POINT('',#11281);
#2770=VERTEX_POINT('',#11288);
#2771=VERTEX_POINT('',#11290);
#2772=VERTEX_POINT('',#11297);
#2773=VERTEX_POINT('',#11299);
#2774=VERTEX_POINT('',#11306);
#2775=VERTEX_POINT('',#11319);
#2776=VERTEX_POINT('',#11320);
#2777=VERTEX_POINT('',#11322);
#2778=VERTEX_POINT('',#11329);
#2779=VERTEX_POINT('',#11331);
#2780=VERTEX_POINT('',#11338);
#2781=VERTEX_POINT('',#11340);
#2782=VERTEX_POINT('',#11347);
#2783=VERTEX_POINT('',#11500);
#2784=VERTEX_POINT('',#11501);
#2785=VERTEX_POINT('',#11503);
#2786=VERTEX_POINT('',#11505);
#2787=VERTEX_POINT('',#11509);
#2788=VERTEX_POINT('',#11510);
#2789=VERTEX_POINT('',#11515);
#2790=VERTEX_POINT('',#11519);
#2791=VERTEX_POINT('',#11526);
#2792=VERTEX_POINT('',#11527);
#2793=VERTEX_POINT('',#11529);
#2794=VERTEX_POINT('',#11531);
#2795=VERTEX_POINT('',#11535);
#2796=VERTEX_POINT('',#11536);
#2797=VERTEX_POINT('',#11541);
#2798=VERTEX_POINT('',#11545);
#2799=VERTEX_POINT('',#11552);
#2800=VERTEX_POINT('',#11553);
#2801=VERTEX_POINT('',#11555);
#2802=VERTEX_POINT('',#11557);
#2803=VERTEX_POINT('',#11561);
#2804=VERTEX_POINT('',#11562);
#2805=VERTEX_POINT('',#11567);
#2806=VERTEX_POINT('',#11571);
#2807=VERTEX_POINT('',#11578);
#2808=VERTEX_POINT('',#11579);
#2809=VERTEX_POINT('',#11581);
#2810=VERTEX_POINT('',#11583);
#2811=VERTEX_POINT('',#11587);
#2812=VERTEX_POINT('',#11588);
#2813=VERTEX_POINT('',#11590);
#2814=VERTEX_POINT('',#11592);
#2815=VERTEX_POINT('',#11596);
#2816=VERTEX_POINT('',#11597);
#2817=VERTEX_POINT('',#11599);
#2818=VERTEX_POINT('',#11601);
#2819=VERTEX_POINT('',#11605);
#2820=VERTEX_POINT('',#11607);
#2821=VERTEX_POINT('',#11610);
#2822=VERTEX_POINT('',#11612);
#2823=VERTEX_POINT('',#11615);
#2824=VERTEX_POINT('',#11617);
#2825=VERTEX_POINT('',#11620);
#2826=VERTEX_POINT('',#11623);
#2827=VERTEX_POINT('',#11624);
#2828=VERTEX_POINT('',#11626);
#2829=VERTEX_POINT('',#11628);
#2830=VERTEX_POINT('',#11632);
#2831=VERTEX_POINT('',#11633);
#2832=VERTEX_POINT('',#11635);
#2833=VERTEX_POINT('',#11637);
#2834=VERTEX_POINT('',#11641);
#2835=VERTEX_POINT('',#11642);
#2836=VERTEX_POINT('',#11644);
#2837=VERTEX_POINT('',#11646);
#2838=VERTEX_POINT('',#11650);
#2839=VERTEX_POINT('',#11652);
#2840=VERTEX_POINT('',#11655);
#2841=VERTEX_POINT('',#11657);
#2842=VERTEX_POINT('',#11660);
#2843=VERTEX_POINT('',#11662);
#2844=VERTEX_POINT('',#11665);
#2845=VERTEX_POINT('',#11668);
#2846=VERTEX_POINT('',#11669);
#2847=VERTEX_POINT('',#11671);
#2848=VERTEX_POINT('',#11673);
#2849=VERTEX_POINT('',#11677);
#2850=VERTEX_POINT('',#11678);
#2851=VERTEX_POINT('',#11680);
#2852=VERTEX_POINT('',#11682);
#2853=VERTEX_POINT('',#11686);
#2854=VERTEX_POINT('',#11687);
#2855=VERTEX_POINT('',#11689);
#2856=VERTEX_POINT('',#11691);
#2857=VERTEX_POINT('',#11695);
#2858=VERTEX_POINT('',#11697);
#2859=VERTEX_POINT('',#11700);
#2860=VERTEX_POINT('',#11702);
#2861=VERTEX_POINT('',#11705);
#2862=VERTEX_POINT('',#11707);
#2863=VERTEX_POINT('',#11710);
#2864=VERTEX_POINT('',#11713);
#2865=VERTEX_POINT('',#11715);
#2866=VERTEX_POINT('',#11717);
#2867=VERTEX_POINT('',#11732);
#2868=VERTEX_POINT('',#11747);
#2869=VERTEX_POINT('',#11750);
#2870=VERTEX_POINT('',#11779);
#2871=VERTEX_POINT('',#11780);
#2872=VERTEX_POINT('',#11833);
#2873=VERTEX_POINT('',#11834);
#2874=VERTEX_POINT('',#11888);
#2875=VERTEX_POINT('',#11891);
#2876=VERTEX_POINT('',#11894);
#2877=VERTEX_POINT('',#11899);
#2878=VERTEX_POINT('',#11903);
#2879=VERTEX_POINT('',#11905);
#2880=VERTEX_POINT('',#11907);
#2881=VERTEX_POINT('',#11910);
#2882=VERTEX_POINT('',#11912);
#2883=VERTEX_POINT('',#11915);
#2884=VERTEX_POINT('',#11917);
#2885=VERTEX_POINT('',#11921);
#2886=VERTEX_POINT('',#11922);
#2887=VERTEX_POINT('',#11927);
#2888=VERTEX_POINT('',#11928);
#2889=VERTEX_POINT('',#11943);
#2890=VERTEX_POINT('',#11958);
#2891=VERTEX_POINT('',#11991);
#2892=VERTEX_POINT('',#11995);
#2893=VERTEX_POINT('',#11999);
#2894=VERTEX_POINT('',#12001);
#2895=VERTEX_POINT('',#12003);
#2896=VERTEX_POINT('',#12005);
#2897=VERTEX_POINT('',#12008);
#2898=VERTEX_POINT('',#12010);
#2899=VERTEX_POINT('',#12013);
#2900=VERTEX_POINT('',#12017);
#2901=VERTEX_POINT('',#12018);
#2902=VERTEX_POINT('',#12023);
#2903=VERTEX_POINT('',#12025);
#2904=VERTEX_POINT('',#12027);
#2905=VERTEX_POINT('',#12029);
#2906=VERTEX_POINT('',#12032);
#2907=VERTEX_POINT('',#12034);
#2908=VERTEX_POINT('',#12037);
#2909=VERTEX_POINT('',#12041);
#2910=VERTEX_POINT('',#12042);
#2911=VERTEX_POINT('',#12047);
#2912=VERTEX_POINT('',#12048);
#2913=VERTEX_POINT('',#12103);
#2914=VERTEX_POINT('',#12104);
#2915=VERTEX_POINT('',#12163);
#2916=VERTEX_POINT('',#12215);
#2917=VERTEX_POINT('',#12217);
#2918=VERTEX_POINT('',#12221);
#2919=VERTEX_POINT('',#12224);
#2920=VERTEX_POINT('',#12227);
#2921=VERTEX_POINT('',#12229);
#2922=VERTEX_POINT('',#12235);
#2923=VERTEX_POINT('',#12241);
#2924=VERTEX_POINT('',#12243);
#2925=VERTEX_POINT('',#12247);
#2926=VERTEX_POINT('',#12250);
#2927=VERTEX_POINT('',#12253);
#2928=VERTEX_POINT('',#12255);
#2929=VERTEX_POINT('',#12261);
#2930=VERTEX_POINT('',#12267);
#2931=VERTEX_POINT('',#12269);
#2932=VERTEX_POINT('',#12273);
#2933=VERTEX_POINT('',#12276);
#2934=VERTEX_POINT('',#12279);
#2935=VERTEX_POINT('',#12281);
#2936=VERTEX_POINT('',#12287);
#2937=VERTEX_POINT('',#12293);
#2938=VERTEX_POINT('',#12295);
#2939=VERTEX_POINT('',#12299);
#2940=VERTEX_POINT('',#12302);
#2941=VERTEX_POINT('',#12305);
#2942=VERTEX_POINT('',#12307);
#2943=VERTEX_POINT('',#12313);
#2944=VERTEX_POINT('',#12319);
#2945=VERTEX_POINT('',#12320);
#2946=VERTEX_POINT('',#12322);
#2947=VERTEX_POINT('',#12324);
#2948=VERTEX_POINT('',#12328);
#2949=VERTEX_POINT('',#12329);
#2950=VERTEX_POINT('',#12331);
#2951=VERTEX_POINT('',#12333);
#2952=VERTEX_POINT('',#12337);
#2953=VERTEX_POINT('',#12338);
#2954=VERTEX_POINT('',#12340);
#2955=VERTEX_POINT('',#12342);
#2956=VERTEX_POINT('',#12346);
#2957=VERTEX_POINT('',#12347);
#2958=VERTEX_POINT('',#12349);
#2959=VERTEX_POINT('',#12358);
#2960=VERTEX_POINT('',#12373);
#2961=VERTEX_POINT('',#12375);
#2962=VERTEX_POINT('',#12399);
#2963=VERTEX_POINT('',#12401);
#2964=VERTEX_POINT('',#12410);
#2965=VERTEX_POINT('',#12445);
#2966=VERTEX_POINT('',#12447);
#2967=VERTEX_POINT('',#12458);
#2968=VERTEX_POINT('',#12491);
#2969=VERTEX_POINT('',#12515);
#2970=VERTEX_POINT('',#12544);
#2971=VERTEX_POINT('',#12545);
#2972=VERTEX_POINT('',#12547);
#2973=VERTEX_POINT('',#12549);
#2974=VERTEX_POINT('',#12553);
#2975=VERTEX_POINT('',#12554);
#2976=VERTEX_POINT('',#12556);
#2977=VERTEX_POINT('',#12565);
#2978=VERTEX_POINT('',#12580);
#2979=VERTEX_POINT('',#12582);
#2980=VERTEX_POINT('',#12606);
#2981=VERTEX_POINT('',#12608);
#2982=VERTEX_POINT('',#12617);
#2983=VERTEX_POINT('',#12652);
#2984=VERTEX_POINT('',#12654);
#2985=VERTEX_POINT('',#12663);
#2986=VERTEX_POINT('',#12698);
#2987=VERTEX_POINT('',#12722);
#2988=VERTEX_POINT('',#12751);
#2989=VERTEX_POINT('',#12752);
#2990=VERTEX_POINT('',#12754);
#2991=VERTEX_POINT('',#12763);
#2992=VERTEX_POINT('',#12778);
#2993=VERTEX_POINT('',#12780);
#2994=VERTEX_POINT('',#12804);
#2995=VERTEX_POINT('',#12806);
#2996=VERTEX_POINT('',#12815);
#2997=VERTEX_POINT('',#12850);
#2998=VERTEX_POINT('',#12852);
#2999=VERTEX_POINT('',#12863);
#3000=VERTEX_POINT('',#12896);
#3001=VERTEX_POINT('',#12920);
#3002=VERTEX_POINT('',#12949);
#3003=VERTEX_POINT('',#12950);
#3004=VERTEX_POINT('',#12952);
#3005=VERTEX_POINT('',#12954);
#3006=VERTEX_POINT('',#12958);
#3007=VERTEX_POINT('',#12959);
#3008=VERTEX_POINT('',#12961);
#3009=VERTEX_POINT('',#12963);
#3010=VERTEX_POINT('',#12967);
#3011=VERTEX_POINT('',#12969);
#3012=VERTEX_POINT('',#12971);
#3013=VERTEX_POINT('',#12974);
#3014=VERTEX_POINT('',#12976);
#3015=VERTEX_POINT('',#12979);
#3016=VERTEX_POINT('',#12981);
#3017=VERTEX_POINT('',#12985);
#3018=VERTEX_POINT('',#12987);
#3019=VERTEX_POINT('',#12989);
#3020=VERTEX_POINT('',#12992);
#3021=VERTEX_POINT('',#12994);
#3022=VERTEX_POINT('',#12997);
#3023=VERTEX_POINT('',#12999);
#3024=VERTEX_POINT('',#13005);
#3025=VERTEX_POINT('',#13007);
#3026=VERTEX_POINT('',#13010);
#3027=VERTEX_POINT('',#13012);
#3028=VERTEX_POINT('',#13015);
#3029=VERTEX_POINT('',#13017);
#3030=VERTEX_POINT('',#13020);
#3031=VERTEX_POINT('',#13023);
#3032=VERTEX_POINT('',#13025);
#3033=VERTEX_POINT('',#13028);
#3034=VERTEX_POINT('',#13030);
#3035=VERTEX_POINT('',#13033);
#3036=VERTEX_POINT('',#13035);
#3037=VERTEX_POINT('',#13039);
#3038=VERTEX_POINT('',#13041);
#3039=VERTEX_POINT('',#13045);
#3040=VERTEX_POINT('',#13047);
#3041=VERTEX_POINT('',#13068);
#3042=VERTEX_POINT('',#13070);
#3043=VERTEX_POINT('',#13075);
#3044=VERTEX_POINT('',#13077);
#3045=VERTEX_POINT('',#13082);
#3046=VERTEX_POINT('',#13084);
#3047=VERTEX_POINT('',#13089);
#3048=VERTEX_POINT('',#13091);
#3049=VERTEX_POINT('',#13096);
#3050=VERTEX_POINT('',#13098);
#3051=VERTEX_POINT('',#13103);
#3052=VERTEX_POINT('',#13105);
#3053=VERTEX_POINT('',#13110);
#3054=VERTEX_POINT('',#13113);
#3055=VERTEX_POINT('',#13114);
#3056=VERTEX_POINT('',#13160);
#3057=VERTEX_POINT('',#13161);
#3058=VERTEX_POINT('',#13207);
#3059=VERTEX_POINT('',#13208);
#3060=VERTEX_POINT('',#13250);
#3061=VERTEX_POINT('',#13251);
#3062=VERTEX_POINT('',#13293);
#3063=VERTEX_POINT('',#13294);
#3064=VERTEX_POINT('',#13336);
#3065=VERTEX_POINT('',#13337);
#3066=VERTEX_POINT('',#13379);
#3067=VERTEX_POINT('',#13380);
#3068=VERTEX_POINT('',#13422);
#3069=VERTEX_POINT('',#13423);
#3070=VERTEX_POINT('',#13465);
#3071=VERTEX_POINT('',#13466);
#3072=VERTEX_POINT('',#13512);
#3073=VERTEX_POINT('',#13513);
#3074=VERTEX_POINT('',#13555);
#3075=VERTEX_POINT('',#13556);
#3076=VERTEX_POINT('',#13598);
#3077=VERTEX_POINT('',#13599);
#3078=VERTEX_POINT('',#13643);
#3079=VERTEX_POINT('',#13645);
#3080=VERTEX_POINT('',#13658);
#3081=VERTEX_POINT('',#13660);
#3082=VERTEX_POINT('',#13664);
#3083=VERTEX_POINT('',#13666);
#3084=VERTEX_POINT('',#13687);
#3085=VERTEX_POINT('',#13689);
#3086=VERTEX_POINT('',#13693);
#3087=VERTEX_POINT('',#13695);
#3088=VERTEX_POINT('',#13716);
#3089=VERTEX_POINT('',#13718);
#3090=VERTEX_POINT('',#13723);
#3091=VERTEX_POINT('',#13725);
#3092=VERTEX_POINT('',#13730);
#3093=VERTEX_POINT('',#13732);
#3094=VERTEX_POINT('',#13737);
#3095=VERTEX_POINT('',#13739);
#3096=VERTEX_POINT('',#13744);
#3097=VERTEX_POINT('',#13746);
#3098=VERTEX_POINT('',#13751);
#3099=VERTEX_POINT('',#13753);
#3100=VERTEX_POINT('',#13758);
#3101=VERTEX_POINT('',#13762);
#3102=VERTEX_POINT('',#13766);
#3103=VERTEX_POINT('',#13770);
#3104=VERTEX_POINT('',#13774);
#3105=VERTEX_POINT('',#13778);
#3106=VERTEX_POINT('',#13782);
#3107=VERTEX_POINT('',#13786);
#3108=VERTEX_POINT('',#13790);
#3109=VERTEX_POINT('',#13795);
#3110=VERTEX_POINT('',#13800);
#3111=VERTEX_POINT('',#13805);
#3112=VERTEX_POINT('',#13810);
#3113=VERTEX_POINT('',#13815);
#3114=VERTEX_POINT('',#13820);
#3115=VERTEX_POINT('',#13825);
#3116=VERTEX_POINT('',#13834);
#3117=VERTEX_POINT('',#13838);
#3118=VERTEX_POINT('',#13897);
#3119=VERTEX_POINT('',#13901);
#3120=VERTEX_POINT('',#13960);
#3121=VERTEX_POINT('',#13964);
#3122=VERTEX_POINT('',#14075);
#3123=VERTEX_POINT('',#14077);
#3124=VERTEX_POINT('',#14081);
#3125=VERTEX_POINT('',#14084);
#3126=VERTEX_POINT('',#14087);
#3127=VERTEX_POINT('',#14091);
#3128=EDGE_CURVE('',#2579,#2580,#1803,.T.);
#3129=EDGE_CURVE('',#2580,#2581,#1804,.T.);
#3130=EDGE_CURVE('',#2582,#2581,#1805,.T.);
#3131=EDGE_CURVE('',#2582,#2583,#1806,.T.);
#3132=EDGE_CURVE('',#2583,#2584,#1807,.T.);
#3133=EDGE_CURVE('',#2584,#2585,#1543,.T.);
#3134=EDGE_CURVE('',#2585,#2586,#1808,.T.);
#3135=EDGE_CURVE('',#2579,#2586,#1809,.T.);
#3136=EDGE_CURVE('',#2587,#2587,#1544,.T.);
#3137=EDGE_CURVE('',#2588,#2588,#1545,.T.);
#3138=EDGE_CURVE('',#2589,#2589,#1546,.T.);
#3139=EDGE_CURVE('',#2590,#2591,#1547,.T.);
#3140=EDGE_CURVE('',#2592,#2590,#1548,.T.);
#3141=EDGE_CURVE('',#2592,#2593,#1549,.T.);
#3142=EDGE_CURVE('',#2594,#2593,#1550,.T.);
#3143=EDGE_CURVE('',#2595,#2594,#1551,.T.);
#3144=EDGE_CURVE('',#2596,#2595,#1552,.T.);
#3145=EDGE_CURVE('',#2596,#2597,#1553,.T.);
#3146=EDGE_CURVE('',#2597,#2591,#1554,.T.);
#3147=EDGE_CURVE('',#2598,#2599,#1810,.T.);
#3148=EDGE_CURVE('',#2600,#2598,#1811,.T.);
#3149=EDGE_CURVE('',#2601,#2600,#1812,.T.);
#3150=EDGE_CURVE('',#2599,#2601,#1813,.T.);
#3151=EDGE_CURVE('',#2602,#2602,#1555,.F.);
#3152=EDGE_CURVE('',#2603,#2603,#1556,.F.);
#3153=EDGE_CURVE('',#2604,#2604,#1557,.F.);
#3154=EDGE_CURVE('',#2605,#2605,#1558,.T.);
#3155=EDGE_CURVE('',#2606,#2606,#1559,.T.);
#3156=EDGE_CURVE('',#2607,#2607,#1560,.T.);
#3157=EDGE_CURVE('',#2608,#2609,#1814,.T.);
#3158=EDGE_CURVE('',#2609,#2610,#1815,.T.);
#3159=EDGE_CURVE('',#2610,#2611,#1816,.T.);
#3160=EDGE_CURVE('',#2611,#2608,#1817,.T.);
#3161=EDGE_CURVE('',#2612,#2612,#1561,.F.);
#3162=EDGE_CURVE('',#2612,#2613,#1818,.T.);
#3163=EDGE_CURVE('',#2613,#2613,#1562,.T.);
#3164=EDGE_CURVE('',#2614,#2615,#292,.T.);
#3165=EDGE_CURVE('',#2615,#2614,#293,.T.);
#3166=EDGE_CURVE('',#2616,#2617,#294,.T.);
#3167=EDGE_CURVE('',#2617,#2616,#295,.T.);
#3168=EDGE_CURVE('',#2618,#2618,#1563,.T.);
#3169=EDGE_CURVE('',#2618,#2617,#1819,.T.);
#3170=EDGE_CURVE('',#2619,#2620,#1820,.T.);
#3171=EDGE_CURVE('',#2621,#2620,#296,.T.);
#3172=EDGE_CURVE('',#2622,#2621,#297,.T.);
#3173=EDGE_CURVE('',#2623,#2622,#1821,.T.);
#3174=EDGE_CURVE('',#2623,#2624,#1564,.T.);
#3175=EDGE_CURVE('',#2624,#2625,#1822,.T.);
#3176=EDGE_CURVE('',#2626,#2625,#298,.T.);
#3177=EDGE_CURVE('',#2627,#2626,#1823,.T.);
#3178=EDGE_CURVE('',#2627,#2619,#1565,.T.);
#3179=EDGE_CURVE('',#2628,#2629,#1824,.T.);
#3180=EDGE_CURVE('',#2628,#2630,#1825,.T.);
#3181=EDGE_CURVE('',#2631,#2630,#1826,.F.);
#3182=EDGE_CURVE('',#2631,#2632,#1827,.T.);
#3183=EDGE_CURVE('',#2632,#2633,#1566,.T.);
#3184=EDGE_CURVE('',#2633,#2634,#1828,.T.);
#3185=EDGE_CURVE('',#2634,#2635,#1829,.F.);
#3186=EDGE_CURVE('',#2629,#2635,#1830,.T.);
#3187=EDGE_CURVE('',#2636,#2636,#1567,.T.);
#3188=EDGE_CURVE('',#2637,#2637,#1568,.T.);
#3189=EDGE_CURVE('',#2638,#2638,#1569,.T.);
#3190=EDGE_CURVE('',#2639,#2640,#1570,.T.);
#3191=EDGE_CURVE('',#2599,#2640,#1831,.T.);
#3192=EDGE_CURVE('',#2601,#2580,#1832,.T.);
#3193=EDGE_CURVE('',#2579,#2639,#299,.T.);
#3194=EDGE_CURVE('',#2611,#2628,#1833,.T.);
#3195=EDGE_CURVE('',#2641,#2610,#1834,.T.);
#3196=EDGE_CURVE('',#2641,#2642,#1571,.T.);
#3197=EDGE_CURVE('',#2642,#2630,#300,.T.);
#3198=EDGE_CURVE('',#2600,#2581,#1835,.T.);
#3199=EDGE_CURVE('',#2619,#2598,#1836,.T.);
#3200=EDGE_CURVE('',#2582,#2627,#301,.F.);
#3201=EDGE_CURVE('',#2609,#2623,#1837,.T.);
#3202=EDGE_CURVE('',#2608,#2629,#1838,.T.);
#3203=EDGE_CURVE('',#2624,#2635,#302,.F.);
#3204=EDGE_CURVE('',#2643,#2583,#303,.T.);
#3205=EDGE_CURVE('',#2643,#2584,#1839,.T.);
#3206=EDGE_CURVE('',#2644,#2633,#1840,.T.);
#3207=EDGE_CURVE('',#2644,#2634,#304,.T.);
#3208=EDGE_CURVE('',#2645,#2646,#305,.T.);
#3209=EDGE_CURVE('',#2595,#2645,#1841,.T.);
#3210=EDGE_CURVE('',#2594,#2646,#1842,.T.);
#3211=EDGE_CURVE('',#2647,#2648,#306,.T.);
#3212=EDGE_CURVE('',#2593,#2648,#1843,.T.);
#3213=EDGE_CURVE('',#2592,#2647,#1844,.T.);
#3214=EDGE_CURVE('',#2646,#2648,#307,.T.);
#3215=EDGE_CURVE('',#2649,#2631,#308,.T.);
#3216=EDGE_CURVE('',#2649,#2648,#1845,.T.);
#3217=EDGE_CURVE('',#2647,#2631,#309,.T.);
#3218=EDGE_CURVE('',#2645,#2586,#310,.T.);
#3219=EDGE_CURVE('',#2646,#2650,#1846,.T.);
#3220=EDGE_CURVE('',#2586,#2650,#311,.T.);
#3221=EDGE_CURVE('',#2650,#2649,#312,.T.);
#3222=EDGE_CURVE('',#2639,#2650,#1847,.T.);
#3223=EDGE_CURVE('',#2622,#2641,#1848,.T.);
#3224=EDGE_CURVE('',#2620,#2622,#313,.T.);
#3225=EDGE_CURVE('',#2620,#2640,#1849,.T.);
#3226=EDGE_CURVE('',#2642,#2649,#1850,.T.);
#3227=EDGE_CURVE('',#2645,#2585,#1851,.T.);
#3228=EDGE_CURVE('',#2647,#2632,#1852,.T.);
#3229=EDGE_CURVE('',#2596,#2643,#1853,.T.);
#3230=EDGE_CURVE('',#2590,#2644,#1854,.T.);
#3231=EDGE_CURVE('',#2643,#2651,#314,.T.);
#3232=EDGE_CURVE('',#2597,#2651,#1855,.T.);
#3233=EDGE_CURVE('',#2644,#2652,#315,.T.);
#3234=EDGE_CURVE('',#2591,#2652,#1856,.T.);
#3235=EDGE_CURVE('',#2651,#2652,#316,.T.);
#3236=EDGE_CURVE('',#2625,#2634,#317,.T.);
#3237=EDGE_CURVE('',#2625,#2652,#1857,.T.);
#3238=EDGE_CURVE('',#2583,#2626,#318,.T.);
#3239=EDGE_CURVE('',#2651,#2626,#1858,.T.);
#3240=EDGE_CURVE('',#2653,#2620,#1572,.T.);
#3241=EDGE_CURVE('',#2620,#2653,#1573,.T.);
#3242=EDGE_CURVE('',#2622,#2654,#1574,.T.);
#3243=EDGE_CURVE('',#2654,#2622,#1575,.T.);
#3244=EDGE_CURVE('',#2653,#2655,#1859,.T.);
#3245=EDGE_CURVE('',#2655,#2655,#1576,.T.);
#3246=EDGE_CURVE('',#2656,#2656,#1577,.T.);
#3247=EDGE_CURVE('',#2654,#2657,#1860,.T.);
#3248=EDGE_CURVE('',#2657,#2657,#1578,.T.);
#3249=EDGE_CURVE('',#2615,#2656,#1861,.T.);
#3250=EDGE_CURVE('',#2658,#2658,#1579,.T.);
#3251=EDGE_CURVE('',#2658,#2621,#1862,.T.);
#3252=EDGE_CURVE('',#2607,#2589,#1863,.T.);
#3253=EDGE_CURVE('',#2606,#2588,#1864,.T.);
#3254=EDGE_CURVE('',#2605,#2587,#1865,.T.);
#3255=EDGE_CURVE('',#2604,#2638,#1866,.T.);
#3256=EDGE_CURVE('',#2603,#2637,#1867,.T.);
#3257=EDGE_CURVE('',#2602,#2636,#1868,.T.);
#3258=EDGE_CURVE('',#2659,#2660,#1580,.T.);
#3259=EDGE_CURVE('',#2660,#2659,#1581,.T.);
#3260=EDGE_CURVE('',#2659,#2661,#1869,.T.);
#3261=EDGE_CURVE('',#2662,#2661,#319,.T.);
#3262=EDGE_CURVE('',#2663,#2662,#320,.T.);
#3263=EDGE_CURVE('',#2663,#2664,#1870,.T.);
#3264=EDGE_CURVE('',#2664,#2665,#1582,.F.);
#3265=EDGE_CURVE('',#2665,#2664,#1583,.F.);
#3266=EDGE_CURVE('',#2661,#2663,#321,.T.);
#3267=EDGE_CURVE('',#2666,#2667,#1871,.F.);
#3268=EDGE_CURVE('',#2667,#2668,#1584,.T.);
#3269=EDGE_CURVE('',#2668,#2669,#1872,.T.);
#3270=EDGE_CURVE('',#2669,#2666,#1585,.F.);
#3271=EDGE_CURVE('',#2670,#2671,#1873,.F.);
#3272=EDGE_CURVE('',#2671,#2672,#1586,.T.);
#3273=EDGE_CURVE('',#2672,#2673,#1874,.T.);
#3274=EDGE_CURVE('',#2673,#2670,#1587,.F.);
#3275=EDGE_CURVE('',#2674,#2675,#1875,.F.);
#3276=EDGE_CURVE('',#2675,#2676,#1588,.T.);
#3277=EDGE_CURVE('',#2676,#2677,#1876,.T.);
#3278=EDGE_CURVE('',#2677,#2674,#1589,.F.);
#3279=EDGE_CURVE('',#2678,#2679,#1877,.F.);
#3280=EDGE_CURVE('',#2679,#2680,#1590,.T.);
#3281=EDGE_CURVE('',#2680,#2681,#1878,.T.);
#3282=EDGE_CURVE('',#2681,#2678,#1591,.F.);
#3283=EDGE_CURVE('',#2682,#2682,#322,.T.);
#3284=EDGE_CURVE('',#2683,#2683,#323,.T.);
#3285=EDGE_CURVE('',#2684,#2684,#324,.T.);
#3286=EDGE_CURVE('',#2685,#2685,#1592,.T.);
#3287=EDGE_CURVE('',#2686,#2686,#1593,.F.);
#3288=EDGE_CURVE('',#2687,#2687,#1594,.F.);
#3289=EDGE_CURVE('',#2688,#2689,#1595,.T.);
#3290=EDGE_CURVE('',#2688,#2690,#325,.T.);
#3291=EDGE_CURVE('',#2690,#2691,#1879,.T.);
#3292=EDGE_CURVE('',#2691,#2692,#326,.T.);
#3293=EDGE_CURVE('',#2692,#2693,#1596,.T.);
#3294=EDGE_CURVE('',#2693,#2694,#327,.T.);
#3295=EDGE_CURVE('',#2694,#2695,#1880,.F.);
#3296=EDGE_CURVE('',#2695,#2689,#328,.T.);
#3297=EDGE_CURVE('',#2689,#2688,#1597,.F.);
#3298=EDGE_CURVE('',#2692,#2693,#1598,.T.);
#3299=EDGE_CURVE('',#2681,#2694,#329,.F.);
#3300=EDGE_CURVE('',#2695,#2680,#330,.T.);
#3301=EDGE_CURVE('',#2690,#2679,#331,.T.);
#3302=EDGE_CURVE('',#2678,#2691,#332,.F.);
#3303=EDGE_CURVE('',#2696,#2697,#1599,.T.);
#3304=EDGE_CURVE('',#2696,#2698,#333,.T.);
#3305=EDGE_CURVE('',#2698,#2699,#1881,.T.);
#3306=EDGE_CURVE('',#2699,#2700,#334,.T.);
#3307=EDGE_CURVE('',#2700,#2701,#1600,.T.);
#3308=EDGE_CURVE('',#2701,#2702,#335,.T.);
#3309=EDGE_CURVE('',#2702,#2703,#1882,.F.);
#3310=EDGE_CURVE('',#2703,#2697,#336,.T.);
#3311=EDGE_CURVE('',#2697,#2696,#1601,.F.);
#3312=EDGE_CURVE('',#2700,#2701,#1602,.T.);
#3313=EDGE_CURVE('',#2704,#2705,#1603,.T.);
#3314=EDGE_CURVE('',#2704,#2706,#337,.T.);
#3315=EDGE_CURVE('',#2706,#2707,#1883,.T.);
#3316=EDGE_CURVE('',#2707,#2708,#338,.T.);
#3317=EDGE_CURVE('',#2708,#2709,#1604,.T.);
#3318=EDGE_CURVE('',#2709,#2710,#339,.T.);
#3319=EDGE_CURVE('',#2710,#2711,#1884,.F.);
#3320=EDGE_CURVE('',#2711,#2705,#340,.T.);
#3321=EDGE_CURVE('',#2705,#2704,#1605,.F.);
#3322=EDGE_CURVE('',#2708,#2709,#1606,.T.);
#3323=EDGE_CURVE('',#2712,#2713,#1607,.T.);
#3324=EDGE_CURVE('',#2712,#2714,#341,.T.);
#3325=EDGE_CURVE('',#2714,#2715,#1885,.T.);
#3326=EDGE_CURVE('',#2715,#2716,#342,.T.);
#3327=EDGE_CURVE('',#2716,#2717,#1608,.T.);
#3328=EDGE_CURVE('',#2717,#2718,#343,.T.);
#3329=EDGE_CURVE('',#2718,#2719,#1886,.F.);
#3330=EDGE_CURVE('',#2719,#2713,#344,.T.);
#3331=EDGE_CURVE('',#2713,#2712,#1609,.F.);
#3332=EDGE_CURVE('',#2716,#2717,#1610,.T.);
#3333=EDGE_CURVE('',#2677,#2718,#345,.F.);
#3334=EDGE_CURVE('',#2719,#2676,#346,.T.);
#3335=EDGE_CURVE('',#2714,#2675,#347,.T.);
#3336=EDGE_CURVE('',#2674,#2715,#348,.F.);
#3337=EDGE_CURVE('',#2673,#2710,#349,.F.);
#3338=EDGE_CURVE('',#2711,#2672,#350,.T.);
#3339=EDGE_CURVE('',#2706,#2671,#351,.T.);
#3340=EDGE_CURVE('',#2670,#2707,#352,.F.);
#3341=EDGE_CURVE('',#2669,#2702,#353,.F.);
#3342=EDGE_CURVE('',#2703,#2668,#354,.T.);
#3343=EDGE_CURVE('',#2698,#2667,#355,.T.);
#3344=EDGE_CURVE('',#2666,#2699,#356,.F.);
#3345=EDGE_CURVE('',#2660,#2686,#1611,.T.);
#3346=EDGE_CURVE('',#2685,#2665,#1612,.T.);
#3347=EDGE_CURVE('',#2687,#2720,#1887,.T.);
#3348=EDGE_CURVE('',#2720,#2720,#1613,.T.);
#3349=EDGE_CURVE('',#2721,#2722,#1614,.T.);
#3350=EDGE_CURVE('',#2722,#2721,#1615,.T.);
#3351=EDGE_CURVE('',#2721,#2723,#1888,.T.);
#3352=EDGE_CURVE('',#2724,#2723,#357,.T.);
#3353=EDGE_CURVE('',#2725,#2724,#358,.T.);
#3354=EDGE_CURVE('',#2725,#2726,#1889,.T.);
#3355=EDGE_CURVE('',#2726,#2727,#1616,.F.);
#3356=EDGE_CURVE('',#2727,#2726,#1617,.F.);
#3357=EDGE_CURVE('',#2723,#2725,#359,.T.);
#3358=EDGE_CURVE('',#2728,#2729,#1890,.F.);
#3359=EDGE_CURVE('',#2729,#2730,#1618,.T.);
#3360=EDGE_CURVE('',#2730,#2731,#1891,.T.);
#3361=EDGE_CURVE('',#2731,#2728,#1619,.F.);
#3362=EDGE_CURVE('',#2732,#2733,#1892,.F.);
#3363=EDGE_CURVE('',#2733,#2734,#1620,.T.);
#3364=EDGE_CURVE('',#2734,#2735,#1893,.T.);
#3365=EDGE_CURVE('',#2735,#2732,#1621,.F.);
#3366=EDGE_CURVE('',#2736,#2737,#1894,.F.);
#3367=EDGE_CURVE('',#2737,#2738,#1622,.T.);
#3368=EDGE_CURVE('',#2738,#2739,#1895,.T.);
#3369=EDGE_CURVE('',#2739,#2736,#1623,.F.);
#3370=EDGE_CURVE('',#2740,#2741,#1896,.F.);
#3371=EDGE_CURVE('',#2741,#2742,#1624,.T.);
#3372=EDGE_CURVE('',#2742,#2743,#1897,.T.);
#3373=EDGE_CURVE('',#2743,#2740,#1625,.F.);
#3374=EDGE_CURVE('',#2744,#2744,#360,.T.);
#3375=EDGE_CURVE('',#2745,#2745,#361,.T.);
#3376=EDGE_CURVE('',#2746,#2746,#362,.T.);
#3377=EDGE_CURVE('',#2747,#2747,#1626,.T.);
#3378=EDGE_CURVE('',#2748,#2748,#1627,.T.);
#3379=EDGE_CURVE('',#2749,#2749,#1628,.F.);
#3380=EDGE_CURVE('',#2750,#2750,#1629,.T.);
#3381=EDGE_CURVE('',#2751,#2752,#1630,.T.);
#3382=EDGE_CURVE('',#2751,#2753,#363,.T.);
#3383=EDGE_CURVE('',#2753,#2754,#1898,.T.);
#3384=EDGE_CURVE('',#2754,#2755,#364,.T.);
#3385=EDGE_CURVE('',#2755,#2756,#1631,.T.);
#3386=EDGE_CURVE('',#2756,#2757,#365,.T.);
#3387=EDGE_CURVE('',#2757,#2758,#1899,.F.);
#3388=EDGE_CURVE('',#2758,#2752,#366,.T.);
#3389=EDGE_CURVE('',#2752,#2751,#1632,.F.);
#3390=EDGE_CURVE('',#2755,#2756,#1633,.T.);
#3391=EDGE_CURVE('',#2743,#2757,#367,.F.);
#3392=EDGE_CURVE('',#2758,#2742,#368,.T.);
#3393=EDGE_CURVE('',#2753,#2741,#369,.T.);
#3394=EDGE_CURVE('',#2740,#2754,#370,.F.);
#3395=EDGE_CURVE('',#2759,#2760,#1634,.T.);
#3396=EDGE_CURVE('',#2759,#2761,#371,.T.);
#3397=EDGE_CURVE('',#2761,#2762,#1900,.T.);
#3398=EDGE_CURVE('',#2762,#2763,#372,.T.);
#3399=EDGE_CURVE('',#2763,#2764,#1635,.T.);
#3400=EDGE_CURVE('',#2764,#2765,#373,.T.);
#3401=EDGE_CURVE('',#2765,#2766,#1901,.F.);
#3402=EDGE_CURVE('',#2766,#2760,#374,.T.);
#3403=EDGE_CURVE('',#2760,#2759,#1636,.F.);
#3404=EDGE_CURVE('',#2763,#2764,#1637,.T.);
#3405=EDGE_CURVE('',#2767,#2768,#1638,.T.);
#3406=EDGE_CURVE('',#2767,#2769,#375,.T.);
#3407=EDGE_CURVE('',#2769,#2770,#1902,.T.);
#3408=EDGE_CURVE('',#2770,#2771,#376,.T.);
#3409=EDGE_CURVE('',#2771,#2772,#1639,.T.);
#3410=EDGE_CURVE('',#2772,#2773,#377,.T.);
#3411=EDGE_CURVE('',#2773,#2774,#1903,.F.);
#3412=EDGE_CURVE('',#2774,#2768,#378,.T.);
#3413=EDGE_CURVE('',#2768,#2767,#1640,.F.);
#3414=EDGE_CURVE('',#2771,#2772,#1641,.T.);
#3415=EDGE_CURVE('',#2775,#2776,#1642,.T.);
#3416=EDGE_CURVE('',#2775,#2777,#379,.T.);
#3417=EDGE_CURVE('',#2777,#2778,#1904,.T.);
#3418=EDGE_CURVE('',#2778,#2779,#380,.T.);
#3419=EDGE_CURVE('',#2779,#2780,#1643,.T.);
#3420=EDGE_CURVE('',#2780,#2781,#381,.T.);
#3421=EDGE_CURVE('',#2781,#2782,#1905,.F.);
#3422=EDGE_CURVE('',#2782,#2776,#382,.T.);
#3423=EDGE_CURVE('',#2776,#2775,#1644,.F.);
#3424=EDGE_CURVE('',#2779,#2780,#1645,.T.);
#3425=EDGE_CURVE('',#2739,#2781,#383,.F.);
#3426=EDGE_CURVE('',#2782,#2738,#384,.T.);
#3427=EDGE_CURVE('',#2777,#2737,#385,.T.);
#3428=EDGE_CURVE('',#2736,#2778,#386,.F.);
#3429=EDGE_CURVE('',#2735,#2773,#387,.F.);
#3430=EDGE_CURVE('',#2774,#2734,#388,.T.);
#3431=EDGE_CURVE('',#2769,#2733,#389,.T.);
#3432=EDGE_CURVE('',#2732,#2770,#390,.F.);
#3433=EDGE_CURVE('',#2731,#2765,#391,.F.);
#3434=EDGE_CURVE('',#2766,#2730,#392,.T.);
#3435=EDGE_CURVE('',#2761,#2729,#393,.T.);
#3436=EDGE_CURVE('',#2728,#2762,#394,.F.);
#3437=EDGE_CURVE('',#2722,#2749,#1646,.T.);
#3438=EDGE_CURVE('',#2747,#2727,#1647,.T.);
#3439=EDGE_CURVE('',#2750,#2748,#1906,.T.);
#3440=EDGE_CURVE('',#2783,#2784,#1648,.T.);
#3441=EDGE_CURVE('',#2784,#2785,#1907,.T.);
#3442=EDGE_CURVE('',#2785,#2786,#1649,.T.);
#3443=EDGE_CURVE('',#2786,#2783,#1908,.T.);
#3444=EDGE_CURVE('',#2787,#2788,#1909,.T.);
#3445=EDGE_CURVE('',#2787,#2785,#1910,.T.);
#3446=EDGE_CURVE('',#2788,#2784,#1911,.T.);
#3447=EDGE_CURVE('',#2789,#2787,#1650,.T.);
#3448=EDGE_CURVE('',#2789,#2786,#1912,.T.);
#3449=EDGE_CURVE('',#2790,#2789,#1913,.T.);
#3450=EDGE_CURVE('',#2790,#2783,#1914,.T.);
#3451=EDGE_CURVE('',#2788,#2790,#1651,.F.);
#3452=EDGE_CURVE('',#2791,#2792,#1652,.T.);
#3453=EDGE_CURVE('',#2792,#2793,#1915,.T.);
#3454=EDGE_CURVE('',#2793,#2794,#1653,.T.);
#3455=EDGE_CURVE('',#2794,#2791,#1916,.T.);
#3456=EDGE_CURVE('',#2795,#2796,#1917,.T.);
#3457=EDGE_CURVE('',#2795,#2793,#1918,.T.);
#3458=EDGE_CURVE('',#2796,#2792,#1919,.T.);
#3459=EDGE_CURVE('',#2797,#2795,#1654,.T.);
#3460=EDGE_CURVE('',#2797,#2794,#1920,.T.);
#3461=EDGE_CURVE('',#2798,#2797,#1921,.T.);
#3462=EDGE_CURVE('',#2798,#2791,#1922,.T.);
#3463=EDGE_CURVE('',#2796,#2798,#1655,.F.);
#3464=EDGE_CURVE('',#2799,#2800,#1656,.T.);
#3465=EDGE_CURVE('',#2800,#2801,#1923,.T.);
#3466=EDGE_CURVE('',#2801,#2802,#1657,.T.);
#3467=EDGE_CURVE('',#2802,#2799,#1924,.T.);
#3468=EDGE_CURVE('',#2803,#2804,#1925,.T.);
#3469=EDGE_CURVE('',#2803,#2801,#1926,.T.);
#3470=EDGE_CURVE('',#2804,#2800,#1927,.T.);
#3471=EDGE_CURVE('',#2805,#2803,#1658,.T.);
#3472=EDGE_CURVE('',#2805,#2802,#1928,.T.);
#3473=EDGE_CURVE('',#2806,#2805,#1929,.T.);
#3474=EDGE_CURVE('',#2806,#2799,#1930,.T.);
#3475=EDGE_CURVE('',#2804,#2806,#1659,.F.);
#3476=EDGE_CURVE('',#2807,#2808,#1931,.T.);
#3477=EDGE_CURVE('',#2809,#2807,#1660,.T.);
#3478=EDGE_CURVE('',#2810,#2809,#1932,.F.);
#3479=EDGE_CURVE('',#2810,#2808,#1661,.T.);
#3480=EDGE_CURVE('',#2811,#2812,#1933,.F.);
#3481=EDGE_CURVE('',#2811,#2813,#1662,.T.);
#3482=EDGE_CURVE('',#2814,#2813,#1934,.T.);
#3483=EDGE_CURVE('',#2812,#2814,#1663,.T.);
#3484=EDGE_CURVE('',#2815,#2816,#1935,.F.);
#3485=EDGE_CURVE('',#2815,#2817,#1664,.T.);
#3486=EDGE_CURVE('',#2818,#2817,#1936,.T.);
#3487=EDGE_CURVE('',#2816,#2818,#1665,.T.);
#3488=EDGE_CURVE('',#2807,#2819,#1937,.T.);
#3489=EDGE_CURVE('',#2820,#2819,#1938,.T.);
#3490=EDGE_CURVE('',#2820,#2812,#1939,.T.);
#3491=EDGE_CURVE('',#2814,#2821,#1940,.T.);
#3492=EDGE_CURVE('',#2822,#2821,#1941,.T.);
#3493=EDGE_CURVE('',#2822,#2816,#1942,.T.);
#3494=EDGE_CURVE('',#2818,#2823,#1943,.T.);
#3495=EDGE_CURVE('',#2824,#2823,#1944,.T.);
#3496=EDGE_CURVE('',#2824,#2809,#1945,.T.);
#3497=EDGE_CURVE('',#2825,#2825,#1666,.F.);
#3498=EDGE_CURVE('',#2826,#2827,#1946,.T.);
#3499=EDGE_CURVE('',#2828,#2826,#1667,.T.);
#3500=EDGE_CURVE('',#2829,#2828,#1947,.F.);
#3501=EDGE_CURVE('',#2829,#2827,#1668,.T.);
#3502=EDGE_CURVE('',#2830,#2831,#1948,.F.);
#3503=EDGE_CURVE('',#2830,#2832,#1669,.T.);
#3504=EDGE_CURVE('',#2833,#2832,#1949,.T.);
#3505=EDGE_CURVE('',#2831,#2833,#1670,.T.);
#3506=EDGE_CURVE('',#2834,#2835,#1950,.F.);
#3507=EDGE_CURVE('',#2834,#2836,#1671,.T.);
#3508=EDGE_CURVE('',#2837,#2836,#1951,.T.);
#3509=EDGE_CURVE('',#2835,#2837,#1672,.T.);
#3510=EDGE_CURVE('',#2826,#2838,#1952,.T.);
#3511=EDGE_CURVE('',#2839,#2838,#1953,.T.);
#3512=EDGE_CURVE('',#2839,#2831,#1954,.T.);
#3513=EDGE_CURVE('',#2833,#2840,#1955,.T.);
#3514=EDGE_CURVE('',#2841,#2840,#1956,.T.);
#3515=EDGE_CURVE('',#2841,#2835,#1957,.T.);
#3516=EDGE_CURVE('',#2837,#2842,#1958,.T.);
#3517=EDGE_CURVE('',#2843,#2842,#1959,.T.);
#3518=EDGE_CURVE('',#2843,#2828,#1960,.T.);
#3519=EDGE_CURVE('',#2844,#2844,#1673,.F.);
#3520=EDGE_CURVE('',#2845,#2846,#1961,.T.);
#3521=EDGE_CURVE('',#2847,#2845,#1674,.T.);
#3522=EDGE_CURVE('',#2848,#2847,#1962,.F.);
#3523=EDGE_CURVE('',#2848,#2846,#1675,.T.);
#3524=EDGE_CURVE('',#2849,#2850,#1963,.F.);
#3525=EDGE_CURVE('',#2849,#2851,#1676,.T.);
#3526=EDGE_CURVE('',#2852,#2851,#1964,.T.);
#3527=EDGE_CURVE('',#2850,#2852,#1677,.T.);
#3528=EDGE_CURVE('',#2853,#2854,#1965,.F.);
#3529=EDGE_CURVE('',#2853,#2855,#1678,.T.);
#3530=EDGE_CURVE('',#2856,#2855,#1966,.T.);
#3531=EDGE_CURVE('',#2854,#2856,#1679,.T.);
#3532=EDGE_CURVE('',#2845,#2857,#1967,.T.);
#3533=EDGE_CURVE('',#2858,#2857,#1968,.T.);
#3534=EDGE_CURVE('',#2858,#2850,#1969,.T.);
#3535=EDGE_CURVE('',#2852,#2859,#1970,.T.);
#3536=EDGE_CURVE('',#2860,#2859,#1971,.T.);
#3537=EDGE_CURVE('',#2860,#2854,#1972,.T.);
#3538=EDGE_CURVE('',#2856,#2861,#1973,.T.);
#3539=EDGE_CURVE('',#2862,#2861,#1974,.T.);
#3540=EDGE_CURVE('',#2862,#2847,#1975,.T.);
#3541=EDGE_CURVE('',#2863,#2863,#1680,.F.);
#3542=EDGE_CURVE('',#2864,#2864,#1681,.T.);
#3543=EDGE_CURVE('',#2864,#2865,#1976,.T.);
#3544=EDGE_CURVE('',#2866,#2865,#395,.T.);
#3545=EDGE_CURVE('',#2867,#2866,#396,.T.);
#3546=EDGE_CURVE('',#2867,#2868,#1977,.T.);
#3547=EDGE_CURVE('',#2868,#2868,#1682,.T.);
#3548=EDGE_CURVE('',#2869,#2867,#397,.T.);
#3549=EDGE_CURVE('',#2865,#2869,#398,.T.);
#3550=EDGE_CURVE('',#2870,#2871,#399,.T.);
#3551=EDGE_CURVE('',#2871,#2870,#400,.T.);
#3552=EDGE_CURVE('',#2872,#2873,#401,.T.);
#3553=EDGE_CURVE('',#2873,#2872,#402,.T.);
#3554=EDGE_CURVE('',#2874,#2874,#1683,.T.);
#3555=EDGE_CURVE('',#2875,#2875,#1684,.T.);
#3556=EDGE_CURVE('',#2876,#2876,#1685,.T.);
#3557=EDGE_CURVE('',#2876,#2874,#1978,.T.);
#3558=EDGE_CURVE('',#2877,#2877,#1686,.T.);
#3559=EDGE_CURVE('',#2877,#2866,#1979,.T.);
#3560=EDGE_CURVE('',#2878,#2878,#1687,.T.);
#3561=EDGE_CURVE('',#2879,#2849,#1980,.T.);
#3562=EDGE_CURVE('',#2879,#2880,#1981,.T.);
#3563=EDGE_CURVE('',#2880,#2846,#1982,.T.);
#3564=EDGE_CURVE('',#2881,#2848,#1983,.T.);
#3565=EDGE_CURVE('',#2881,#2882,#1984,.T.);
#3566=EDGE_CURVE('',#2882,#2855,#1985,.T.);
#3567=EDGE_CURVE('',#2883,#2853,#1986,.T.);
#3568=EDGE_CURVE('',#2883,#2884,#1987,.T.);
#3569=EDGE_CURVE('',#2884,#2851,#1988,.T.);
#3570=EDGE_CURVE('',#2885,#2886,#1688,.T.);
#3571=EDGE_CURVE('',#2886,#2885,#1689,.T.);
#3572=EDGE_CURVE('',#2885,#2878,#1989,.T.);
#3573=EDGE_CURVE('',#2887,#2888,#403,.T.);
#3574=EDGE_CURVE('',#2889,#2887,#404,.T.);
#3575=EDGE_CURVE('',#2890,#2889,#405,.T.);
#3576=EDGE_CURVE('',#2890,#2863,#1990,.T.);
#3577=EDGE_CURVE('',#2888,#2890,#406,.T.);
#3578=EDGE_CURVE('',#2886,#2877,#1991,.T.);
#3579=EDGE_CURVE('',#2891,#2891,#1690,.T.);
#3580=EDGE_CURVE('',#2891,#2873,#1992,.T.);
#3581=EDGE_CURVE('',#2892,#2892,#1691,.T.);
#3582=EDGE_CURVE('',#2892,#2871,#1993,.T.);
#3583=EDGE_CURVE('',#2893,#2893,#1692,.T.);
#3584=EDGE_CURVE('',#2894,#2808,#1994,.T.);
#3585=EDGE_CURVE('',#2895,#2810,#1995,.T.);
#3586=EDGE_CURVE('',#2895,#2896,#1996,.T.);
#3587=EDGE_CURVE('',#2896,#2817,#1997,.T.);
#3588=EDGE_CURVE('',#2897,#2815,#1998,.T.);
#3589=EDGE_CURVE('',#2897,#2898,#1999,.T.);
#3590=EDGE_CURVE('',#2898,#2813,#2000,.T.);
#3591=EDGE_CURVE('',#2899,#2811,#2001,.T.);
#3592=EDGE_CURVE('',#2899,#2894,#2002,.T.);
#3593=EDGE_CURVE('',#2900,#2901,#1693,.T.);
#3594=EDGE_CURVE('',#2901,#2900,#1694,.T.);
#3595=EDGE_CURVE('',#2900,#2893,#2003,.T.);
#3596=EDGE_CURVE('',#2902,#2902,#1695,.T.);
#3597=EDGE_CURVE('',#2903,#2827,#2004,.T.);
#3598=EDGE_CURVE('',#2904,#2829,#2005,.T.);
#3599=EDGE_CURVE('',#2904,#2905,#2006,.T.);
#3600=EDGE_CURVE('',#2905,#2836,#2007,.T.);
#3601=EDGE_CURVE('',#2906,#2834,#2008,.T.);
#3602=EDGE_CURVE('',#2906,#2907,#2009,.T.);
#3603=EDGE_CURVE('',#2907,#2832,#2010,.T.);
#3604=EDGE_CURVE('',#2908,#2830,#2011,.T.);
#3605=EDGE_CURVE('',#2908,#2903,#2012,.T.);
#3606=EDGE_CURVE('',#2909,#2910,#1696,.T.);
#3607=EDGE_CURVE('',#2910,#2909,#1697,.T.);
#3608=EDGE_CURVE('',#2909,#2902,#2013,.T.);
#3609=EDGE_CURVE('',#2911,#2912,#407,.T.);
#3610=EDGE_CURVE('',#2912,#2911,#408,.T.);
#3611=EDGE_CURVE('',#2912,#2825,#2014,.T.);
#3612=EDGE_CURVE('',#2913,#2914,#409,.T.);
#3613=EDGE_CURVE('',#2914,#2913,#410,.T.);
#3614=EDGE_CURVE('',#2914,#2844,#2015,.T.);
#3615=EDGE_CURVE('',#2910,#2891,#2016,.T.);
#3616=EDGE_CURVE('',#2901,#2892,#2017,.T.);
#3617=EDGE_CURVE('',#2915,#2915,#1698,.F.);
#3618=EDGE_CURVE('',#2915,#2888,#2018,.T.);
#3619=EDGE_CURVE('',#2889,#2875,#2019,.T.);
#3620=EDGE_CURVE('',#2882,#2861,#2020,.T.);
#3621=EDGE_CURVE('',#2862,#2881,#2021,.T.);
#3622=EDGE_CURVE('',#2884,#2859,#2022,.T.);
#3623=EDGE_CURVE('',#2860,#2883,#2023,.T.);
#3624=EDGE_CURVE('',#2880,#2857,#2024,.T.);
#3625=EDGE_CURVE('',#2858,#2879,#2025,.T.);
#3626=EDGE_CURVE('',#2905,#2842,#2026,.T.);
#3627=EDGE_CURVE('',#2843,#2904,#2027,.T.);
#3628=EDGE_CURVE('',#2907,#2840,#2028,.T.);
#3629=EDGE_CURVE('',#2841,#2906,#2029,.T.);
#3630=EDGE_CURVE('',#2903,#2838,#2030,.T.);
#3631=EDGE_CURVE('',#2839,#2908,#2031,.T.);
#3632=EDGE_CURVE('',#2896,#2823,#2032,.T.);
#3633=EDGE_CURVE('',#2824,#2895,#2033,.T.);
#3634=EDGE_CURVE('',#2898,#2821,#2034,.T.);
#3635=EDGE_CURVE('',#2822,#2897,#2035,.T.);
#3636=EDGE_CURVE('',#2894,#2819,#2036,.T.);
#3637=EDGE_CURVE('',#2820,#2899,#2037,.T.);
#3638=EDGE_CURVE('',#2916,#2916,#1699,.T.);
#3639=EDGE_CURVE('',#2916,#2917,#2038,.T.);
#3640=EDGE_CURVE('',#2917,#2917,#1700,.T.);
#3641=EDGE_CURVE('',#2918,#2918,#1701,.T.);
#3642=EDGE_CURVE('',#2919,#2919,#1702,.T.);
#3643=EDGE_CURVE('',#2920,#2920,#1703,.T.);
#3644=EDGE_CURVE('',#2920,#2921,#2039,.T.);
#3645=EDGE_CURVE('',#2921,#2921,#1704,.T.);
#3646=EDGE_CURVE('',#2921,#2919,#2040,.T.);
#3647=EDGE_CURVE('',#2922,#2922,#1705,.T.);
#3648=EDGE_CURVE('',#2918,#2922,#2041,.T.);
#3649=EDGE_CURVE('',#2923,#2923,#1706,.T.);
#3650=EDGE_CURVE('',#2923,#2924,#2042,.T.);
#3651=EDGE_CURVE('',#2924,#2924,#1707,.T.);
#3652=EDGE_CURVE('',#2925,#2925,#1708,.T.);
#3653=EDGE_CURVE('',#2926,#2926,#1709,.T.);
#3654=EDGE_CURVE('',#2927,#2927,#1710,.T.);
#3655=EDGE_CURVE('',#2927,#2928,#2043,.T.);
#3656=EDGE_CURVE('',#2928,#2928,#1711,.T.);
#3657=EDGE_CURVE('',#2928,#2926,#2044,.T.);
#3658=EDGE_CURVE('',#2929,#2929,#1712,.T.);
#3659=EDGE_CURVE('',#2925,#2929,#2045,.T.);
#3660=EDGE_CURVE('',#2930,#2930,#1713,.T.);
#3661=EDGE_CURVE('',#2930,#2931,#2046,.T.);
#3662=EDGE_CURVE('',#2931,#2931,#1714,.T.);
#3663=EDGE_CURVE('',#2932,#2932,#1715,.T.);
#3664=EDGE_CURVE('',#2933,#2933,#1716,.T.);
#3665=EDGE_CURVE('',#2934,#2934,#1717,.T.);
#3666=EDGE_CURVE('',#2934,#2935,#2047,.T.);
#3667=EDGE_CURVE('',#2935,#2935,#1718,.T.);
#3668=EDGE_CURVE('',#2935,#2933,#2048,.T.);
#3669=EDGE_CURVE('',#2936,#2936,#1719,.T.);
#3670=EDGE_CURVE('',#2932,#2936,#2049,.T.);
#3671=EDGE_CURVE('',#2937,#2937,#1720,.T.);
#3672=EDGE_CURVE('',#2937,#2938,#2050,.T.);
#3673=EDGE_CURVE('',#2938,#2938,#1721,.T.);
#3674=EDGE_CURVE('',#2939,#2939,#1722,.T.);
#3675=EDGE_CURVE('',#2940,#2940,#1723,.T.);
#3676=EDGE_CURVE('',#2941,#2941,#1724,.T.);
#3677=EDGE_CURVE('',#2941,#2942,#2051,.T.);
#3678=EDGE_CURVE('',#2942,#2942,#1725,.T.);
#3679=EDGE_CURVE('',#2942,#2940,#2052,.T.);
#3680=EDGE_CURVE('',#2943,#2943,#1726,.T.);
#3681=EDGE_CURVE('',#2939,#2943,#2053,.T.);
#3682=EDGE_CURVE('',#2944,#2945,#2054,.F.);
#3683=EDGE_CURVE('',#2946,#2944,#1727,.T.);
#3684=EDGE_CURVE('',#2947,#2946,#2055,.T.);
#3685=EDGE_CURVE('',#2947,#2945,#1728,.T.);
#3686=EDGE_CURVE('',#2948,#2949,#2056,.T.);
#3687=EDGE_CURVE('',#2948,#2950,#1729,.T.);
#3688=EDGE_CURVE('',#2951,#2950,#2057,.F.);
#3689=EDGE_CURVE('',#2949,#2951,#1730,.T.);
#3690=EDGE_CURVE('',#2952,#2953,#1731,.T.);
#3691=EDGE_CURVE('',#2953,#2954,#2058,.F.);
#3692=EDGE_CURVE('',#2955,#2954,#1732,.T.);
#3693=EDGE_CURVE('',#2955,#2952,#2059,.T.);
#3694=EDGE_CURVE('',#2956,#2957,#2060,.T.);
#3695=EDGE_CURVE('',#2958,#2956,#411,.T.);
#3696=EDGE_CURVE('',#2959,#2958,#412,.T.);
#3697=EDGE_CURVE('',#2960,#2959,#2061,.F.);
#3698=EDGE_CURVE('',#2961,#2960,#413,.T.);
#3699=EDGE_CURVE('',#2957,#2961,#414,.T.);
#3700=EDGE_CURVE('',#2962,#2956,#2062,.T.);
#3701=EDGE_CURVE('',#2963,#2962,#415,.T.);
#3702=EDGE_CURVE('',#2964,#2963,#416,.T.);
#3703=EDGE_CURVE('',#2959,#2964,#2063,.F.);
#3704=EDGE_CURVE('',#2956,#2959,#417,.T.);
#3705=EDGE_CURVE('',#2965,#2962,#2064,.T.);
#3706=EDGE_CURVE('',#2966,#2965,#418,.T.);
#3707=EDGE_CURVE('',#2967,#2966,#419,.T.);
#3708=EDGE_CURVE('',#2964,#2967,#2065,.F.);
#3709=EDGE_CURVE('',#2962,#2964,#420,.T.);
#3710=EDGE_CURVE('',#2967,#2968,#2066,.F.);
#3711=EDGE_CURVE('',#2965,#2967,#421,.T.);
#3712=EDGE_CURVE('',#2969,#2965,#2067,.T.);
#3713=EDGE_CURVE('',#2968,#2969,#422,.T.);
#3714=EDGE_CURVE('',#2970,#2971,#1733,.T.);
#3715=EDGE_CURVE('',#2971,#2972,#2068,.F.);
#3716=EDGE_CURVE('',#2973,#2972,#1734,.T.);
#3717=EDGE_CURVE('',#2973,#2970,#2069,.T.);
#3718=EDGE_CURVE('',#2974,#2975,#2070,.T.);
#3719=EDGE_CURVE('',#2976,#2974,#423,.T.);
#3720=EDGE_CURVE('',#2977,#2976,#424,.T.);
#3721=EDGE_CURVE('',#2978,#2977,#2071,.F.);
#3722=EDGE_CURVE('',#2979,#2978,#425,.T.);
#3723=EDGE_CURVE('',#2975,#2979,#426,.T.);
#3724=EDGE_CURVE('',#2980,#2974,#2072,.T.);
#3725=EDGE_CURVE('',#2981,#2980,#427,.T.);
#3726=EDGE_CURVE('',#2982,#2981,#428,.T.);
#3727=EDGE_CURVE('',#2977,#2982,#2073,.F.);
#3728=EDGE_CURVE('',#2974,#2977,#429,.T.);
#3729=EDGE_CURVE('',#2983,#2980,#2074,.T.);
#3730=EDGE_CURVE('',#2984,#2983,#430,.T.);
#3731=EDGE_CURVE('',#2985,#2984,#431,.T.);
#3732=EDGE_CURVE('',#2982,#2985,#2075,.F.);
#3733=EDGE_CURVE('',#2980,#2982,#432,.T.);
#3734=EDGE_CURVE('',#2985,#2986,#2076,.F.);
#3735=EDGE_CURVE('',#2983,#2985,#433,.T.);
#3736=EDGE_CURVE('',#2987,#2983,#2077,.T.);
#3737=EDGE_CURVE('',#2986,#2987,#434,.T.);
#3738=EDGE_CURVE('',#2988,#2989,#2078,.T.);
#3739=EDGE_CURVE('',#2990,#2988,#435,.T.);
#3740=EDGE_CURVE('',#2991,#2990,#436,.T.);
#3741=EDGE_CURVE('',#2992,#2991,#2079,.F.);
#3742=EDGE_CURVE('',#2993,#2992,#437,.T.);
#3743=EDGE_CURVE('',#2989,#2993,#438,.T.);
#3744=EDGE_CURVE('',#2994,#2988,#2080,.T.);
#3745=EDGE_CURVE('',#2995,#2994,#439,.T.);
#3746=EDGE_CURVE('',#2996,#2995,#440,.T.);
#3747=EDGE_CURVE('',#2991,#2996,#2081,.F.);
#3748=EDGE_CURVE('',#2988,#2991,#441,.T.);
#3749=EDGE_CURVE('',#2997,#2994,#2082,.T.);
#3750=EDGE_CURVE('',#2998,#2997,#442,.T.);
#3751=EDGE_CURVE('',#2999,#2998,#443,.T.);
#3752=EDGE_CURVE('',#2996,#2999,#2083,.F.);
#3753=EDGE_CURVE('',#2994,#2996,#444,.T.);
#3754=EDGE_CURVE('',#2999,#3000,#2084,.F.);
#3755=EDGE_CURVE('',#2997,#2999,#445,.T.);
#3756=EDGE_CURVE('',#3001,#2997,#2085,.T.);
#3757=EDGE_CURVE('',#3000,#3001,#446,.T.);
#3758=EDGE_CURVE('',#3002,#3003,#1735,.T.);
#3759=EDGE_CURVE('',#3002,#3004,#2086,.T.);
#3760=EDGE_CURVE('',#3004,#3005,#1736,.T.);
#3761=EDGE_CURVE('',#3005,#3003,#2087,.F.);
#3762=EDGE_CURVE('',#3006,#3007,#2088,.T.);
#3763=EDGE_CURVE('',#3006,#3008,#1737,.T.);
#3764=EDGE_CURVE('',#3009,#3008,#2089,.F.);
#3765=EDGE_CURVE('',#3007,#3009,#1738,.T.);
#3766=EDGE_CURVE('',#3010,#3010,#1739,.T.);
#3767=EDGE_CURVE('',#3011,#3004,#2090,.T.);
#3768=EDGE_CURVE('',#3012,#3011,#1740,.F.);
#3769=EDGE_CURVE('',#3012,#2953,#2091,.T.);
#3770=EDGE_CURVE('',#3013,#2952,#2092,.T.);
#3771=EDGE_CURVE('',#3014,#3013,#1741,.F.);
#3772=EDGE_CURVE('',#3014,#2971,#2093,.T.);
#3773=EDGE_CURVE('',#3015,#2970,#2094,.T.);
#3774=EDGE_CURVE('',#3016,#3015,#1742,.F.);
#3775=EDGE_CURVE('',#3016,#3005,#2095,.T.);
#3776=EDGE_CURVE('',#3017,#3017,#1743,.T.);
#3777=EDGE_CURVE('',#3018,#2944,#2096,.T.);
#3778=EDGE_CURVE('',#3019,#3018,#2097,.T.);
#3779=EDGE_CURVE('',#2949,#3019,#2098,.T.);
#3780=EDGE_CURVE('',#3020,#2951,#2099,.T.);
#3781=EDGE_CURVE('',#3021,#3020,#2100,.T.);
#3782=EDGE_CURVE('',#3007,#3021,#2101,.T.);
#3783=EDGE_CURVE('',#3022,#3009,#2102,.T.);
#3784=EDGE_CURVE('',#3023,#3022,#2103,.T.);
#3785=EDGE_CURVE('',#2946,#3023,#2104,.T.);
#3786=EDGE_CURVE('',#3017,#3010,#2105,.T.);
#3787=EDGE_CURVE('',#2948,#3024,#2106,.T.);
#3788=EDGE_CURVE('',#3024,#3025,#2107,.T.);
#3789=EDGE_CURVE('',#3025,#2945,#2108,.T.);
#3790=EDGE_CURVE('',#2947,#3026,#2109,.T.);
#3791=EDGE_CURVE('',#3026,#3027,#2110,.T.);
#3792=EDGE_CURVE('',#3027,#3008,#2111,.T.);
#3793=EDGE_CURVE('',#3006,#3028,#2112,.T.);
#3794=EDGE_CURVE('',#3028,#3029,#2113,.T.);
#3795=EDGE_CURVE('',#3029,#2950,#2114,.T.);
#3796=EDGE_CURVE('',#3030,#3030,#1744,.T.);
#3797=EDGE_CURVE('',#3031,#2954,#2115,.T.);
#3798=EDGE_CURVE('',#3032,#3031,#1745,.F.);
#3799=EDGE_CURVE('',#3002,#3032,#2116,.T.);
#3800=EDGE_CURVE('',#3033,#3003,#2117,.T.);
#3801=EDGE_CURVE('',#3034,#3033,#1746,.F.);
#3802=EDGE_CURVE('',#2973,#3034,#2118,.T.);
#3803=EDGE_CURVE('',#3035,#2972,#2119,.T.);
#3804=EDGE_CURVE('',#3036,#3035,#1747,.F.);
#3805=EDGE_CURVE('',#2955,#3036,#2120,.T.);
#3806=EDGE_CURVE('',#3037,#3037,#1748,.T.);
#3807=EDGE_CURVE('',#3038,#3038,#1749,.T.);
#3808=EDGE_CURVE('',#3037,#2993,#2121,.T.);
#3809=EDGE_CURVE('',#3039,#2992,#2122,.T.);
#3810=EDGE_CURVE('',#3039,#3040,#447,.T.);
#3811=EDGE_CURVE('',#3040,#2989,#2123,.T.);
#3812=EDGE_CURVE('',#3041,#3041,#1750,.T.);
#3813=EDGE_CURVE('',#3042,#3042,#1751,.T.);
#3814=EDGE_CURVE('',#3041,#2990,#2124,.T.);
#3815=EDGE_CURVE('',#3043,#3043,#1752,.T.);
#3816=EDGE_CURVE('',#3044,#3044,#1753,.T.);
#3817=EDGE_CURVE('',#3043,#2995,#2125,.T.);
#3818=EDGE_CURVE('',#3045,#3045,#1754,.T.);
#3819=EDGE_CURVE('',#3046,#3046,#1755,.T.);
#3820=EDGE_CURVE('',#3045,#2998,#2126,.T.);
#3821=EDGE_CURVE('',#3047,#3047,#1756,.T.);
#3822=EDGE_CURVE('',#3048,#3048,#1757,.T.);
#3823=EDGE_CURVE('',#3047,#3038,#2127,.T.);
#3824=EDGE_CURVE('',#3049,#3049,#1758,.T.);
#3825=EDGE_CURVE('',#3050,#3050,#1759,.T.);
#3826=EDGE_CURVE('',#3049,#3042,#2128,.T.);
#3827=EDGE_CURVE('',#3051,#3051,#1760,.T.);
#3828=EDGE_CURVE('',#3052,#3052,#1761,.T.);
#3829=EDGE_CURVE('',#3051,#3044,#2129,.T.);
#3830=EDGE_CURVE('',#3053,#3053,#1762,.F.);
#3831=EDGE_CURVE('',#3053,#3030,#2130,.T.);
#3832=EDGE_CURVE('',#3054,#3055,#448,.T.);
#3833=EDGE_CURVE('',#3055,#3054,#449,.T.);
#3834=EDGE_CURVE('',#3056,#3057,#450,.T.);
#3835=EDGE_CURVE('',#3057,#3056,#451,.T.);
#3836=EDGE_CURVE('',#3058,#3059,#452,.T.);
#3837=EDGE_CURVE('',#3059,#3058,#453,.T.);
#3838=EDGE_CURVE('',#3060,#3061,#454,.T.);
#3839=EDGE_CURVE('',#3061,#3060,#455,.T.);
#3840=EDGE_CURVE('',#3062,#3063,#456,.T.);
#3841=EDGE_CURVE('',#3063,#3062,#457,.T.);
#3842=EDGE_CURVE('',#3064,#3065,#458,.T.);
#3843=EDGE_CURVE('',#3065,#3064,#459,.T.);
#3844=EDGE_CURVE('',#3066,#3067,#460,.T.);
#3845=EDGE_CURVE('',#3067,#3066,#461,.T.);
#3846=EDGE_CURVE('',#3068,#3069,#462,.T.);
#3847=EDGE_CURVE('',#3069,#3068,#463,.T.);
#3848=EDGE_CURVE('',#3070,#3071,#464,.T.);
#3849=EDGE_CURVE('',#3071,#3070,#465,.T.);
#3850=EDGE_CURVE('',#3072,#3073,#466,.T.);
#3851=EDGE_CURVE('',#3073,#3072,#467,.T.);
#3852=EDGE_CURVE('',#3074,#3075,#468,.T.);
#3853=EDGE_CURVE('',#3075,#3074,#469,.T.);
#3854=EDGE_CURVE('',#3076,#3077,#470,.T.);
#3855=EDGE_CURVE('',#3077,#3076,#471,.T.);
#3856=EDGE_CURVE('',#3078,#3078,#1763,.T.);
#3857=EDGE_CURVE('',#3079,#3079,#1764,.T.);
#3858=EDGE_CURVE('',#3078,#3046,#2131,.T.);
#3859=EDGE_CURVE('',#3077,#3048,#2132,.T.);
#3860=EDGE_CURVE('',#3075,#3050,#2133,.T.);
#3861=EDGE_CURVE('',#3073,#3052,#2134,.T.);
#3862=EDGE_CURVE('',#3071,#3079,#2135,.T.);
#3863=EDGE_CURVE('',#3080,#3080,#1765,.T.);
#3864=EDGE_CURVE('',#3081,#3081,#1766,.T.);
#3865=EDGE_CURVE('',#3080,#2961,#2136,.T.);
#3866=EDGE_CURVE('',#3082,#2960,#2137,.T.);
#3867=EDGE_CURVE('',#3082,#3083,#472,.T.);
#3868=EDGE_CURVE('',#3083,#2957,#2138,.T.);
#3869=EDGE_CURVE('',#3084,#3084,#1767,.T.);
#3870=EDGE_CURVE('',#3085,#3085,#1768,.T.);
#3871=EDGE_CURVE('',#3084,#2979,#2139,.T.);
#3872=EDGE_CURVE('',#3086,#2978,#2140,.T.);
#3873=EDGE_CURVE('',#3086,#3087,#473,.T.);
#3874=EDGE_CURVE('',#3087,#2975,#2141,.T.);
#3875=EDGE_CURVE('',#3088,#3088,#1769,.T.);
#3876=EDGE_CURVE('',#3089,#3089,#1770,.T.);
#3877=EDGE_CURVE('',#3088,#2958,#2142,.T.);
#3878=EDGE_CURVE('',#3090,#3090,#1771,.T.);
#3879=EDGE_CURVE('',#3091,#3091,#1772,.T.);
#3880=EDGE_CURVE('',#3090,#2976,#2143,.T.);
#3881=EDGE_CURVE('',#3092,#3092,#1773,.T.);
#3882=EDGE_CURVE('',#3093,#3093,#1774,.T.);
#3883=EDGE_CURVE('',#3092,#2963,#2144,.T.);
#3884=EDGE_CURVE('',#3094,#3094,#1775,.T.);
#3885=EDGE_CURVE('',#3095,#3095,#1776,.T.);
#3886=EDGE_CURVE('',#3094,#2981,#2145,.T.);
#3887=EDGE_CURVE('',#3096,#3096,#1777,.T.);
#3888=EDGE_CURVE('',#3097,#3097,#1778,.T.);
#3889=EDGE_CURVE('',#3096,#2966,#2146,.T.);
#3890=EDGE_CURVE('',#3098,#3098,#1779,.T.);
#3891=EDGE_CURVE('',#3099,#3099,#1780,.T.);
#3892=EDGE_CURVE('',#3098,#2984,#2147,.T.);
#3893=EDGE_CURVE('',#3069,#3100,#2148,.T.);
#3894=EDGE_CURVE('',#3100,#3100,#1781,.F.);
#3895=EDGE_CURVE('',#3067,#3101,#2149,.T.);
#3896=EDGE_CURVE('',#3101,#3101,#1782,.F.);
#3897=EDGE_CURVE('',#3065,#3102,#2150,.T.);
#3898=EDGE_CURVE('',#3102,#3102,#1783,.F.);
#3899=EDGE_CURVE('',#3063,#3103,#2151,.T.);
#3900=EDGE_CURVE('',#3103,#3103,#1784,.F.);
#3901=EDGE_CURVE('',#3061,#3104,#2152,.T.);
#3902=EDGE_CURVE('',#3104,#3104,#1785,.F.);
#3903=EDGE_CURVE('',#3059,#3105,#2153,.T.);
#3904=EDGE_CURVE('',#3105,#3105,#1786,.F.);
#3905=EDGE_CURVE('',#3057,#3106,#2154,.T.);
#3906=EDGE_CURVE('',#3106,#3106,#1787,.F.);
#3907=EDGE_CURVE('',#3055,#3107,#2155,.T.);
#3908=EDGE_CURVE('',#3107,#3107,#1788,.F.);
#3909=EDGE_CURVE('',#3108,#3108,#1789,.T.);
#3910=EDGE_CURVE('',#3108,#3081,#2156,.T.);
#3911=EDGE_CURVE('',#3109,#3109,#1790,.T.);
#3912=EDGE_CURVE('',#3109,#3085,#2157,.T.);
#3913=EDGE_CURVE('',#3110,#3110,#1791,.T.);
#3914=EDGE_CURVE('',#3110,#3089,#2158,.T.);
#3915=EDGE_CURVE('',#3111,#3111,#1792,.T.);
#3916=EDGE_CURVE('',#3111,#3091,#2159,.T.);
#3917=EDGE_CURVE('',#3112,#3112,#1793,.T.);
#3918=EDGE_CURVE('',#3112,#3093,#2160,.T.);
#3919=EDGE_CURVE('',#3113,#3113,#1794,.T.);
#3920=EDGE_CURVE('',#3113,#3095,#2161,.T.);
#3921=EDGE_CURVE('',#3114,#3114,#1795,.T.);
#3922=EDGE_CURVE('',#3114,#3097,#2162,.T.);
#3923=EDGE_CURVE('',#3115,#3115,#1796,.T.);
#3924=EDGE_CURVE('',#3115,#3099,#2163,.T.);
#3925=EDGE_CURVE('',#3033,#3016,#2164,.T.);
#3926=EDGE_CURVE('',#3015,#3034,#2165,.F.);
#3927=EDGE_CURVE('',#3116,#3000,#2166,.T.);
#3928=EDGE_CURVE('',#3116,#3039,#2167,.T.);
#3929=EDGE_CURVE('',#3040,#3117,#2168,.F.);
#3930=EDGE_CURVE('',#3117,#3001,#2169,.T.);
#3931=EDGE_CURVE('',#3117,#3116,#474,.T.);
#3932=EDGE_CURVE('',#3035,#3014,#2170,.T.);
#3933=EDGE_CURVE('',#3013,#3036,#2171,.F.);
#3934=EDGE_CURVE('',#3118,#2986,#2172,.T.);
#3935=EDGE_CURVE('',#3118,#3086,#2173,.T.);
#3936=EDGE_CURVE('',#3087,#3119,#2174,.F.);
#3937=EDGE_CURVE('',#3119,#2987,#2175,.T.);
#3938=EDGE_CURVE('',#3119,#3118,#475,.T.);
#3939=EDGE_CURVE('',#3031,#3012,#2176,.T.);
#3940=EDGE_CURVE('',#3011,#3032,#2177,.F.);
#3941=EDGE_CURVE('',#3120,#2968,#2178,.T.);
#3942=EDGE_CURVE('',#3120,#3082,#2179,.T.);
#3943=EDGE_CURVE('',#3083,#3121,#2180,.F.);
#3944=EDGE_CURVE('',#3121,#2969,#2181,.T.);
#3945=EDGE_CURVE('',#3121,#3120,#476,.T.);
#3946=EDGE_CURVE('',#3027,#3022,#2182,.T.);
#3947=EDGE_CURVE('',#3026,#3023,#2183,.T.);
#3948=EDGE_CURVE('',#3029,#3020,#2184,.T.);
#3949=EDGE_CURVE('',#3028,#3021,#2185,.T.);
#3950=EDGE_CURVE('',#3025,#3018,#2186,.T.);
#3951=EDGE_CURVE('',#3024,#3019,#2187,.T.);
#3952=EDGE_CURVE('',#3122,#3122,#1797,.T.);
#3953=EDGE_CURVE('',#3122,#3123,#2188,.T.);
#3954=EDGE_CURVE('',#3123,#3123,#1798,.T.);
#3955=EDGE_CURVE('',#3124,#3124,#1799,.T.);
#3956=EDGE_CURVE('',#3125,#3125,#1800,.T.);
#3957=EDGE_CURVE('',#3125,#3126,#2189,.T.);
#3958=EDGE_CURVE('',#3126,#3126,#1801,.T.);
#3959=EDGE_CURVE('',#3127,#3127,#1802,.T.);
#3960=EDGE_CURVE('',#3124,#3127,#2190,.T.);
#3961=ORIENTED_EDGE('',*,*,#3128,.T.);
#3962=ORIENTED_EDGE('',*,*,#3129,.T.);
#3963=ORIENTED_EDGE('',*,*,#3130,.F.);
#3964=ORIENTED_EDGE('',*,*,#3131,.T.);
#3965=ORIENTED_EDGE('',*,*,#3132,.T.);
#3966=ORIENTED_EDGE('',*,*,#3133,.T.);
#3967=ORIENTED_EDGE('',*,*,#3134,.T.);
#3968=ORIENTED_EDGE('',*,*,#3135,.F.);
#3969=ORIENTED_EDGE('',*,*,#3136,.F.);
#3970=ORIENTED_EDGE('',*,*,#3137,.F.);
#3971=ORIENTED_EDGE('',*,*,#3138,.F.);
#3972=ORIENTED_EDGE('',*,*,#3139,.F.);
#3973=ORIENTED_EDGE('',*,*,#3140,.F.);
#3974=ORIENTED_EDGE('',*,*,#3141,.T.);
#3975=ORIENTED_EDGE('',*,*,#3142,.F.);
#3976=ORIENTED_EDGE('',*,*,#3143,.F.);
#3977=ORIENTED_EDGE('',*,*,#3144,.F.);
#3978=ORIENTED_EDGE('',*,*,#3145,.T.);
#3979=ORIENTED_EDGE('',*,*,#3146,.T.);
#3980=ORIENTED_EDGE('',*,*,#3147,.F.);
#3981=ORIENTED_EDGE('',*,*,#3148,.F.);
#3982=ORIENTED_EDGE('',*,*,#3149,.F.);
#3983=ORIENTED_EDGE('',*,*,#3150,.F.);
#3984=ORIENTED_EDGE('',*,*,#3151,.T.);
#3985=ORIENTED_EDGE('',*,*,#3152,.T.);
#3986=ORIENTED_EDGE('',*,*,#3153,.T.);
#3987=ORIENTED_EDGE('',*,*,#3154,.F.);
#3988=ORIENTED_EDGE('',*,*,#3155,.F.);
#3989=ORIENTED_EDGE('',*,*,#3156,.F.);
#3990=ORIENTED_EDGE('',*,*,#3157,.T.);
#3991=ORIENTED_EDGE('',*,*,#3158,.T.);
#3992=ORIENTED_EDGE('',*,*,#3159,.T.);
#3993=ORIENTED_EDGE('',*,*,#3160,.T.);
#3994=ORIENTED_EDGE('',*,*,#3161,.F.);
#3995=ORIENTED_EDGE('',*,*,#3162,.T.);
#3996=ORIENTED_EDGE('',*,*,#3163,.T.);
#3997=ORIENTED_EDGE('',*,*,#3162,.F.);
#3998=ORIENTED_EDGE('',*,*,#3164,.T.);
#3999=ORIENTED_EDGE('',*,*,#3165,.T.);
#4000=ORIENTED_EDGE('',*,*,#3166,.T.);
#4001=ORIENTED_EDGE('',*,*,#3167,.T.);
#4002=ORIENTED_EDGE('',*,*,#3168,.T.);
#4003=ORIENTED_EDGE('',*,*,#3169,.T.);
#4004=ORIENTED_EDGE('',*,*,#3166,.F.);
#4005=ORIENTED_EDGE('',*,*,#3167,.F.);
#4006=ORIENTED_EDGE('',*,*,#3169,.F.);
#4007=ORIENTED_EDGE('',*,*,#3170,.T.);
#4008=ORIENTED_EDGE('',*,*,#3171,.F.);
#4009=ORIENTED_EDGE('',*,*,#3172,.F.);
#4010=ORIENTED_EDGE('',*,*,#3173,.F.);
#4011=ORIENTED_EDGE('',*,*,#3174,.T.);
#4012=ORIENTED_EDGE('',*,*,#3175,.T.);
#4013=ORIENTED_EDGE('',*,*,#3176,.F.);
#4014=ORIENTED_EDGE('',*,*,#3177,.F.);
#4015=ORIENTED_EDGE('',*,*,#3178,.T.);
#4016=ORIENTED_EDGE('',*,*,#3179,.F.);
#4017=ORIENTED_EDGE('',*,*,#3180,.T.);
#4018=ORIENTED_EDGE('',*,*,#3181,.F.);
#4019=ORIENTED_EDGE('',*,*,#3182,.T.);
#4020=ORIENTED_EDGE('',*,*,#3183,.T.);
#4021=ORIENTED_EDGE('',*,*,#3184,.T.);
#4022=ORIENTED_EDGE('',*,*,#3185,.T.);
#4023=ORIENTED_EDGE('',*,*,#3186,.F.);
#4024=ORIENTED_EDGE('',*,*,#3187,.T.);
#4025=ORIENTED_EDGE('',*,*,#3188,.T.);
#4026=ORIENTED_EDGE('',*,*,#3189,.T.);
#4027=ORIENTED_EDGE('',*,*,#3190,.T.);
#4028=ORIENTED_EDGE('',*,*,#3191,.F.);
#4029=ORIENTED_EDGE('',*,*,#3150,.T.);
#4030=ORIENTED_EDGE('',*,*,#3192,.T.);
#4031=ORIENTED_EDGE('',*,*,#3128,.F.);
#4032=ORIENTED_EDGE('',*,*,#3193,.T.);
#4033=ORIENTED_EDGE('',*,*,#3180,.F.);
#4034=ORIENTED_EDGE('',*,*,#3194,.F.);
#4035=ORIENTED_EDGE('',*,*,#3159,.F.);
#4036=ORIENTED_EDGE('',*,*,#3195,.F.);
#4037=ORIENTED_EDGE('',*,*,#3196,.T.);
#4038=ORIENTED_EDGE('',*,*,#3197,.T.);
#4039=ORIENTED_EDGE('',*,*,#3130,.T.);
#4040=ORIENTED_EDGE('',*,*,#3198,.F.);
#4041=ORIENTED_EDGE('',*,*,#3148,.T.);
#4042=ORIENTED_EDGE('',*,*,#3199,.F.);
#4043=ORIENTED_EDGE('',*,*,#3178,.F.);
#4044=ORIENTED_EDGE('',*,*,#3200,.F.);
#4045=ORIENTED_EDGE('',*,*,#3174,.F.);
#4046=ORIENTED_EDGE('',*,*,#3201,.F.);
#4047=ORIENTED_EDGE('',*,*,#3157,.F.);
#4048=ORIENTED_EDGE('',*,*,#3202,.T.);
#4049=ORIENTED_EDGE('',*,*,#3186,.T.);
#4050=ORIENTED_EDGE('',*,*,#3203,.F.);
#4051=ORIENTED_EDGE('',*,*,#3132,.F.);
#4052=ORIENTED_EDGE('',*,*,#3204,.F.);
#4053=ORIENTED_EDGE('',*,*,#3205,.T.);
#4054=ORIENTED_EDGE('',*,*,#3206,.F.);
#4055=ORIENTED_EDGE('',*,*,#3207,.T.);
#4056=ORIENTED_EDGE('',*,*,#3184,.F.);
#4057=ORIENTED_EDGE('',*,*,#3208,.F.);
#4058=ORIENTED_EDGE('',*,*,#3209,.F.);
#4059=ORIENTED_EDGE('',*,*,#3143,.T.);
#4060=ORIENTED_EDGE('',*,*,#3210,.T.);
#4061=ORIENTED_EDGE('',*,*,#3211,.T.);
#4062=ORIENTED_EDGE('',*,*,#3212,.F.);
#4063=ORIENTED_EDGE('',*,*,#3141,.F.);
#4064=ORIENTED_EDGE('',*,*,#3213,.T.);
#4065=ORIENTED_EDGE('',*,*,#3214,.F.);
#4066=ORIENTED_EDGE('',*,*,#3210,.F.);
#4067=ORIENTED_EDGE('',*,*,#3142,.T.);
#4068=ORIENTED_EDGE('',*,*,#3212,.T.);
#4069=ORIENTED_EDGE('',*,*,#3215,.F.);
#4070=ORIENTED_EDGE('',*,*,#3216,.T.);
#4071=ORIENTED_EDGE('',*,*,#3211,.F.);
#4072=ORIENTED_EDGE('',*,*,#3217,.T.);
#4073=ORIENTED_EDGE('',*,*,#3218,.F.);
#4074=ORIENTED_EDGE('',*,*,#3208,.T.);
#4075=ORIENTED_EDGE('',*,*,#3219,.T.);
#4076=ORIENTED_EDGE('',*,*,#3220,.F.);
#4077=ORIENTED_EDGE('',*,*,#3221,.F.);
#4078=ORIENTED_EDGE('',*,*,#3219,.F.);
#4079=ORIENTED_EDGE('',*,*,#3214,.T.);
#4080=ORIENTED_EDGE('',*,*,#3216,.F.);
#4081=ORIENTED_EDGE('',*,*,#3193,.F.);
#4082=ORIENTED_EDGE('',*,*,#3135,.T.);
#4083=ORIENTED_EDGE('',*,*,#3220,.T.);
#4084=ORIENTED_EDGE('',*,*,#3222,.F.);
#4085=ORIENTED_EDGE('',*,*,#3223,.F.);
#4086=ORIENTED_EDGE('',*,*,#3224,.F.);
#4087=ORIENTED_EDGE('',*,*,#3225,.T.);
#4088=ORIENTED_EDGE('',*,*,#3190,.F.);
#4089=ORIENTED_EDGE('',*,*,#3222,.T.);
#4090=ORIENTED_EDGE('',*,*,#3221,.T.);
#4091=ORIENTED_EDGE('',*,*,#3226,.F.);
#4092=ORIENTED_EDGE('',*,*,#3196,.F.);
#4093=ORIENTED_EDGE('',*,*,#3215,.T.);
#4094=ORIENTED_EDGE('',*,*,#3181,.T.);
#4095=ORIENTED_EDGE('',*,*,#3197,.F.);
#4096=ORIENTED_EDGE('',*,*,#3226,.T.);
#4097=ORIENTED_EDGE('',*,*,#3218,.T.);
#4098=ORIENTED_EDGE('',*,*,#3134,.F.);
#4099=ORIENTED_EDGE('',*,*,#3227,.F.);
#4100=ORIENTED_EDGE('',*,*,#3217,.F.);
#4101=ORIENTED_EDGE('',*,*,#3228,.T.);
#4102=ORIENTED_EDGE('',*,*,#3182,.F.);
#4103=ORIENTED_EDGE('',*,*,#3133,.F.);
#4104=ORIENTED_EDGE('',*,*,#3205,.F.);
#4105=ORIENTED_EDGE('',*,*,#3229,.F.);
#4106=ORIENTED_EDGE('',*,*,#3144,.T.);
#4107=ORIENTED_EDGE('',*,*,#3209,.T.);
#4108=ORIENTED_EDGE('',*,*,#3227,.T.);
#4109=ORIENTED_EDGE('',*,*,#3183,.F.);
#4110=ORIENTED_EDGE('',*,*,#3228,.F.);
#4111=ORIENTED_EDGE('',*,*,#3213,.F.);
#4112=ORIENTED_EDGE('',*,*,#3140,.T.);
#4113=ORIENTED_EDGE('',*,*,#3230,.T.);
#4114=ORIENTED_EDGE('',*,*,#3206,.T.);
#4115=ORIENTED_EDGE('',*,*,#3231,.T.);
#4116=ORIENTED_EDGE('',*,*,#3232,.F.);
#4117=ORIENTED_EDGE('',*,*,#3145,.F.);
#4118=ORIENTED_EDGE('',*,*,#3229,.T.);
#4119=ORIENTED_EDGE('',*,*,#3233,.F.);
#4120=ORIENTED_EDGE('',*,*,#3230,.F.);
#4121=ORIENTED_EDGE('',*,*,#3139,.T.);
#4122=ORIENTED_EDGE('',*,*,#3234,.T.);
#4123=ORIENTED_EDGE('',*,*,#3235,.T.);
#4124=ORIENTED_EDGE('',*,*,#3234,.F.);
#4125=ORIENTED_EDGE('',*,*,#3146,.F.);
#4126=ORIENTED_EDGE('',*,*,#3232,.T.);
#4127=ORIENTED_EDGE('',*,*,#3236,.T.);
#4128=ORIENTED_EDGE('',*,*,#3207,.F.);
#4129=ORIENTED_EDGE('',*,*,#3233,.T.);
#4130=ORIENTED_EDGE('',*,*,#3237,.F.);
#4131=ORIENTED_EDGE('',*,*,#3204,.T.);
#4132=ORIENTED_EDGE('',*,*,#3238,.T.);
#4133=ORIENTED_EDGE('',*,*,#3239,.F.);
#4134=ORIENTED_EDGE('',*,*,#3231,.F.);
#4135=ORIENTED_EDGE('',*,*,#3176,.T.);
#4136=ORIENTED_EDGE('',*,*,#3237,.T.);
#4137=ORIENTED_EDGE('',*,*,#3235,.F.);
#4138=ORIENTED_EDGE('',*,*,#3239,.T.);
#4139=ORIENTED_EDGE('',*,*,#3131,.F.);
#4140=ORIENTED_EDGE('',*,*,#3200,.T.);
#4141=ORIENTED_EDGE('',*,*,#3177,.T.);
#4142=ORIENTED_EDGE('',*,*,#3238,.F.);
#4143=ORIENTED_EDGE('',*,*,#3185,.F.);
#4144=ORIENTED_EDGE('',*,*,#3236,.F.);
#4145=ORIENTED_EDGE('',*,*,#3175,.F.);
#4146=ORIENTED_EDGE('',*,*,#3203,.T.);
#4147=ORIENTED_EDGE('',*,*,#3225,.F.);
#4148=ORIENTED_EDGE('',*,*,#3240,.F.);
#4149=ORIENTED_EDGE('',*,*,#3241,.F.);
#4150=ORIENTED_EDGE('',*,*,#3170,.F.);
#4151=ORIENTED_EDGE('',*,*,#3199,.T.);
#4152=ORIENTED_EDGE('',*,*,#3147,.T.);
#4153=ORIENTED_EDGE('',*,*,#3191,.T.);
#4154=ORIENTED_EDGE('',*,*,#3173,.T.);
#4155=ORIENTED_EDGE('',*,*,#3242,.T.);
#4156=ORIENTED_EDGE('',*,*,#3243,.T.);
#4157=ORIENTED_EDGE('',*,*,#3223,.T.);
#4158=ORIENTED_EDGE('',*,*,#3195,.T.);
#4159=ORIENTED_EDGE('',*,*,#3158,.F.);
#4160=ORIENTED_EDGE('',*,*,#3201,.T.);
#4161=ORIENTED_EDGE('',*,*,#3241,.T.);
#4162=ORIENTED_EDGE('',*,*,#3244,.T.);
#4163=ORIENTED_EDGE('',*,*,#3245,.F.);
#4164=ORIENTED_EDGE('',*,*,#3244,.F.);
#4165=ORIENTED_EDGE('',*,*,#3240,.T.);
#4166=ORIENTED_EDGE('',*,*,#3245,.T.);
#4167=ORIENTED_EDGE('',*,*,#3246,.F.);
#4168=ORIENTED_EDGE('',*,*,#3242,.F.);
#4169=ORIENTED_EDGE('',*,*,#3243,.F.);
#4170=ORIENTED_EDGE('',*,*,#3247,.T.);
#4171=ORIENTED_EDGE('',*,*,#3248,.T.);
#4172=ORIENTED_EDGE('',*,*,#3247,.F.);
#4173=ORIENTED_EDGE('',*,*,#3248,.F.);
#4174=ORIENTED_EDGE('',*,*,#3168,.F.);
#4175=ORIENTED_EDGE('',*,*,#3164,.F.);
#4176=ORIENTED_EDGE('',*,*,#3165,.F.);
#4177=ORIENTED_EDGE('',*,*,#3249,.T.);
#4178=ORIENTED_EDGE('',*,*,#3246,.T.);
#4179=ORIENTED_EDGE('',*,*,#3249,.F.);
#4180=ORIENTED_EDGE('',*,*,#3250,.T.);
#4181=ORIENTED_EDGE('',*,*,#3163,.F.);
#4182=ORIENTED_EDGE('',*,*,#3250,.F.);
#4183=ORIENTED_EDGE('',*,*,#3251,.T.);
#4184=ORIENTED_EDGE('',*,*,#3171,.T.);
#4185=ORIENTED_EDGE('',*,*,#3224,.T.);
#4186=ORIENTED_EDGE('',*,*,#3172,.T.);
#4187=ORIENTED_EDGE('',*,*,#3251,.F.);
#4188=ORIENTED_EDGE('',*,*,#3161,.T.);
#4189=ORIENTED_EDGE('',*,*,#3179,.T.);
#4190=ORIENTED_EDGE('',*,*,#3202,.F.);
#4191=ORIENTED_EDGE('',*,*,#3160,.F.);
#4192=ORIENTED_EDGE('',*,*,#3194,.T.);
#4193=ORIENTED_EDGE('',*,*,#3129,.F.);
#4194=ORIENTED_EDGE('',*,*,#3192,.F.);
#4195=ORIENTED_EDGE('',*,*,#3149,.T.);
#4196=ORIENTED_EDGE('',*,*,#3198,.T.);
#4197=ORIENTED_EDGE('',*,*,#3156,.T.);
#4198=ORIENTED_EDGE('',*,*,#3252,.T.);
#4199=ORIENTED_EDGE('',*,*,#3138,.T.);
#4200=ORIENTED_EDGE('',*,*,#3252,.F.);
#4201=ORIENTED_EDGE('',*,*,#3155,.T.);
#4202=ORIENTED_EDGE('',*,*,#3253,.T.);
#4203=ORIENTED_EDGE('',*,*,#3137,.T.);
#4204=ORIENTED_EDGE('',*,*,#3253,.F.);
#4205=ORIENTED_EDGE('',*,*,#3154,.T.);
#4206=ORIENTED_EDGE('',*,*,#3254,.T.);
#4207=ORIENTED_EDGE('',*,*,#3136,.T.);
#4208=ORIENTED_EDGE('',*,*,#3254,.F.);
#4209=ORIENTED_EDGE('',*,*,#3153,.F.);
#4210=ORIENTED_EDGE('',*,*,#3255,.T.);
#4211=ORIENTED_EDGE('',*,*,#3189,.F.);
#4212=ORIENTED_EDGE('',*,*,#3255,.F.);
#4213=ORIENTED_EDGE('',*,*,#3152,.F.);
#4214=ORIENTED_EDGE('',*,*,#3256,.T.);
#4215=ORIENTED_EDGE('',*,*,#3188,.F.);
#4216=ORIENTED_EDGE('',*,*,#3256,.F.);
#4217=ORIENTED_EDGE('',*,*,#3151,.F.);
#4218=ORIENTED_EDGE('',*,*,#3257,.T.);
#4219=ORIENTED_EDGE('',*,*,#3187,.F.);
#4220=ORIENTED_EDGE('',*,*,#3257,.F.);
#4221=ORIENTED_EDGE('',*,*,#3258,.T.);
#4222=ORIENTED_EDGE('',*,*,#3259,.T.);
#4223=ORIENTED_EDGE('',*,*,#3260,.T.);
#4224=ORIENTED_EDGE('',*,*,#3261,.F.);
#4225=ORIENTED_EDGE('',*,*,#3262,.F.);
#4226=ORIENTED_EDGE('',*,*,#3263,.T.);
#4227=ORIENTED_EDGE('',*,*,#3264,.T.);
#4228=ORIENTED_EDGE('',*,*,#3265,.T.);
#4229=ORIENTED_EDGE('',*,*,#3263,.F.);
#4230=ORIENTED_EDGE('',*,*,#3266,.F.);
#4231=ORIENTED_EDGE('',*,*,#3260,.F.);
#4232=ORIENTED_EDGE('',*,*,#3267,.T.);
#4233=ORIENTED_EDGE('',*,*,#3268,.T.);
#4234=ORIENTED_EDGE('',*,*,#3269,.T.);
#4235=ORIENTED_EDGE('',*,*,#3270,.T.);
#4236=ORIENTED_EDGE('',*,*,#3271,.T.);
#4237=ORIENTED_EDGE('',*,*,#3272,.T.);
#4238=ORIENTED_EDGE('',*,*,#3273,.T.);
#4239=ORIENTED_EDGE('',*,*,#3274,.T.);
#4240=ORIENTED_EDGE('',*,*,#3275,.T.);
#4241=ORIENTED_EDGE('',*,*,#3276,.T.);
#4242=ORIENTED_EDGE('',*,*,#3277,.T.);
#4243=ORIENTED_EDGE('',*,*,#3278,.T.);
#4244=ORIENTED_EDGE('',*,*,#3279,.T.);
#4245=ORIENTED_EDGE('',*,*,#3280,.T.);
#4246=ORIENTED_EDGE('',*,*,#3281,.T.);
#4247=ORIENTED_EDGE('',*,*,#3282,.T.);
#4248=ORIENTED_EDGE('',*,*,#3283,.F.);
#4249=ORIENTED_EDGE('',*,*,#3284,.F.);
#4250=ORIENTED_EDGE('',*,*,#3285,.F.);
#4251=ORIENTED_EDGE('',*,*,#3286,.T.);
#4252=ORIENTED_EDGE('',*,*,#3287,.T.);
#4253=ORIENTED_EDGE('',*,*,#3288,.F.);
#4254=ORIENTED_EDGE('',*,*,#3283,.T.);
#4255=ORIENTED_EDGE('',*,*,#3284,.T.);
#4256=ORIENTED_EDGE('',*,*,#3285,.T.);
#4257=ORIENTED_EDGE('',*,*,#3261,.T.);
#4258=ORIENTED_EDGE('',*,*,#3266,.T.);
#4259=ORIENTED_EDGE('',*,*,#3262,.T.);
#4260=ORIENTED_EDGE('',*,*,#3289,.F.);
#4261=ORIENTED_EDGE('',*,*,#3290,.T.);
#4262=ORIENTED_EDGE('',*,*,#3291,.T.);
#4263=ORIENTED_EDGE('',*,*,#3292,.T.);
#4264=ORIENTED_EDGE('',*,*,#3293,.T.);
#4265=ORIENTED_EDGE('',*,*,#3294,.T.);
#4266=ORIENTED_EDGE('',*,*,#3295,.T.);
#4267=ORIENTED_EDGE('',*,*,#3296,.T.);
#4268=ORIENTED_EDGE('',*,*,#3289,.T.);
#4269=ORIENTED_EDGE('',*,*,#3297,.T.);
#4270=ORIENTED_EDGE('',*,*,#3293,.F.);
#4271=ORIENTED_EDGE('',*,*,#3298,.T.);
#4272=ORIENTED_EDGE('',*,*,#3299,.F.);
#4273=ORIENTED_EDGE('',*,*,#3281,.F.);
#4274=ORIENTED_EDGE('',*,*,#3300,.F.);
#4275=ORIENTED_EDGE('',*,*,#3295,.F.);
#4276=ORIENTED_EDGE('',*,*,#3300,.T.);
#4277=ORIENTED_EDGE('',*,*,#3280,.F.);
#4278=ORIENTED_EDGE('',*,*,#3301,.F.);
#4279=ORIENTED_EDGE('',*,*,#3290,.F.);
#4280=ORIENTED_EDGE('',*,*,#3297,.F.);
#4281=ORIENTED_EDGE('',*,*,#3296,.F.);
#4282=ORIENTED_EDGE('',*,*,#3298,.F.);
#4283=ORIENTED_EDGE('',*,*,#3292,.F.);
#4284=ORIENTED_EDGE('',*,*,#3302,.F.);
#4285=ORIENTED_EDGE('',*,*,#3282,.F.);
#4286=ORIENTED_EDGE('',*,*,#3299,.T.);
#4287=ORIENTED_EDGE('',*,*,#3294,.F.);
#4288=ORIENTED_EDGE('',*,*,#3301,.T.);
#4289=ORIENTED_EDGE('',*,*,#3279,.F.);
#4290=ORIENTED_EDGE('',*,*,#3302,.T.);
#4291=ORIENTED_EDGE('',*,*,#3291,.F.);
#4292=ORIENTED_EDGE('',*,*,#3303,.F.);
#4293=ORIENTED_EDGE('',*,*,#3304,.T.);
#4294=ORIENTED_EDGE('',*,*,#3305,.T.);
#4295=ORIENTED_EDGE('',*,*,#3306,.T.);
#4296=ORIENTED_EDGE('',*,*,#3307,.T.);
#4297=ORIENTED_EDGE('',*,*,#3308,.T.);
#4298=ORIENTED_EDGE('',*,*,#3309,.T.);
#4299=ORIENTED_EDGE('',*,*,#3310,.T.);
#4300=ORIENTED_EDGE('',*,*,#3303,.T.);
#4301=ORIENTED_EDGE('',*,*,#3311,.T.);
#4302=ORIENTED_EDGE('',*,*,#3307,.F.);
#4303=ORIENTED_EDGE('',*,*,#3312,.T.);
#4304=ORIENTED_EDGE('',*,*,#3313,.F.);
#4305=ORIENTED_EDGE('',*,*,#3314,.T.);
#4306=ORIENTED_EDGE('',*,*,#3315,.T.);
#4307=ORIENTED_EDGE('',*,*,#3316,.T.);
#4308=ORIENTED_EDGE('',*,*,#3317,.T.);
#4309=ORIENTED_EDGE('',*,*,#3318,.T.);
#4310=ORIENTED_EDGE('',*,*,#3319,.T.);
#4311=ORIENTED_EDGE('',*,*,#3320,.T.);
#4312=ORIENTED_EDGE('',*,*,#3313,.T.);
#4313=ORIENTED_EDGE('',*,*,#3321,.T.);
#4314=ORIENTED_EDGE('',*,*,#3317,.F.);
#4315=ORIENTED_EDGE('',*,*,#3322,.T.);
#4316=ORIENTED_EDGE('',*,*,#3323,.F.);
#4317=ORIENTED_EDGE('',*,*,#3324,.T.);
#4318=ORIENTED_EDGE('',*,*,#3325,.T.);
#4319=ORIENTED_EDGE('',*,*,#3326,.T.);
#4320=ORIENTED_EDGE('',*,*,#3327,.T.);
#4321=ORIENTED_EDGE('',*,*,#3328,.T.);
#4322=ORIENTED_EDGE('',*,*,#3329,.T.);
#4323=ORIENTED_EDGE('',*,*,#3330,.T.);
#4324=ORIENTED_EDGE('',*,*,#3323,.T.);
#4325=ORIENTED_EDGE('',*,*,#3331,.T.);
#4326=ORIENTED_EDGE('',*,*,#3327,.F.);
#4327=ORIENTED_EDGE('',*,*,#3332,.T.);
#4328=ORIENTED_EDGE('',*,*,#3333,.F.);
#4329=ORIENTED_EDGE('',*,*,#3277,.F.);
#4330=ORIENTED_EDGE('',*,*,#3334,.F.);
#4331=ORIENTED_EDGE('',*,*,#3329,.F.);
#4332=ORIENTED_EDGE('',*,*,#3334,.T.);
#4333=ORIENTED_EDGE('',*,*,#3276,.F.);
#4334=ORIENTED_EDGE('',*,*,#3335,.F.);
#4335=ORIENTED_EDGE('',*,*,#3324,.F.);
#4336=ORIENTED_EDGE('',*,*,#3331,.F.);
#4337=ORIENTED_EDGE('',*,*,#3330,.F.);
#4338=ORIENTED_EDGE('',*,*,#3332,.F.);
#4339=ORIENTED_EDGE('',*,*,#3326,.F.);
#4340=ORIENTED_EDGE('',*,*,#3336,.F.);
#4341=ORIENTED_EDGE('',*,*,#3278,.F.);
#4342=ORIENTED_EDGE('',*,*,#3333,.T.);
#4343=ORIENTED_EDGE('',*,*,#3328,.F.);
#4344=ORIENTED_EDGE('',*,*,#3335,.T.);
#4345=ORIENTED_EDGE('',*,*,#3275,.F.);
#4346=ORIENTED_EDGE('',*,*,#3336,.T.);
#4347=ORIENTED_EDGE('',*,*,#3325,.F.);
#4348=ORIENTED_EDGE('',*,*,#3337,.F.);
#4349=ORIENTED_EDGE('',*,*,#3273,.F.);
#4350=ORIENTED_EDGE('',*,*,#3338,.F.);
#4351=ORIENTED_EDGE('',*,*,#3319,.F.);
#4352=ORIENTED_EDGE('',*,*,#3338,.T.);
#4353=ORIENTED_EDGE('',*,*,#3272,.F.);
#4354=ORIENTED_EDGE('',*,*,#3339,.F.);
#4355=ORIENTED_EDGE('',*,*,#3314,.F.);
#4356=ORIENTED_EDGE('',*,*,#3321,.F.);
#4357=ORIENTED_EDGE('',*,*,#3320,.F.);
#4358=ORIENTED_EDGE('',*,*,#3322,.F.);
#4359=ORIENTED_EDGE('',*,*,#3316,.F.);
#4360=ORIENTED_EDGE('',*,*,#3340,.F.);
#4361=ORIENTED_EDGE('',*,*,#3274,.F.);
#4362=ORIENTED_EDGE('',*,*,#3337,.T.);
#4363=ORIENTED_EDGE('',*,*,#3318,.F.);
#4364=ORIENTED_EDGE('',*,*,#3339,.T.);
#4365=ORIENTED_EDGE('',*,*,#3271,.F.);
#4366=ORIENTED_EDGE('',*,*,#3340,.T.);
#4367=ORIENTED_EDGE('',*,*,#3315,.F.);
#4368=ORIENTED_EDGE('',*,*,#3341,.F.);
#4369=ORIENTED_EDGE('',*,*,#3269,.F.);
#4370=ORIENTED_EDGE('',*,*,#3342,.F.);
#4371=ORIENTED_EDGE('',*,*,#3309,.F.);
#4372=ORIENTED_EDGE('',*,*,#3342,.T.);
#4373=ORIENTED_EDGE('',*,*,#3268,.F.);
#4374=ORIENTED_EDGE('',*,*,#3343,.F.);
#4375=ORIENTED_EDGE('',*,*,#3304,.F.);
#4376=ORIENTED_EDGE('',*,*,#3311,.F.);
#4377=ORIENTED_EDGE('',*,*,#3310,.F.);
#4378=ORIENTED_EDGE('',*,*,#3312,.F.);
#4379=ORIENTED_EDGE('',*,*,#3306,.F.);
#4380=ORIENTED_EDGE('',*,*,#3344,.F.);
#4381=ORIENTED_EDGE('',*,*,#3270,.F.);
#4382=ORIENTED_EDGE('',*,*,#3341,.T.);
#4383=ORIENTED_EDGE('',*,*,#3308,.F.);
#4384=ORIENTED_EDGE('',*,*,#3343,.T.);
#4385=ORIENTED_EDGE('',*,*,#3267,.F.);
#4386=ORIENTED_EDGE('',*,*,#3344,.T.);
#4387=ORIENTED_EDGE('',*,*,#3305,.F.);
#4388=ORIENTED_EDGE('',*,*,#3258,.F.);
#4389=ORIENTED_EDGE('',*,*,#3259,.F.);
#4390=ORIENTED_EDGE('',*,*,#3345,.T.);
#4391=ORIENTED_EDGE('',*,*,#3287,.F.);
#4392=ORIENTED_EDGE('',*,*,#3345,.F.);
#4393=ORIENTED_EDGE('',*,*,#3286,.F.);
#4394=ORIENTED_EDGE('',*,*,#3346,.T.);
#4395=ORIENTED_EDGE('',*,*,#3264,.F.);
#4396=ORIENTED_EDGE('',*,*,#3265,.F.);
#4397=ORIENTED_EDGE('',*,*,#3346,.F.);
#4398=ORIENTED_EDGE('',*,*,#3288,.T.);
#4399=ORIENTED_EDGE('',*,*,#3347,.T.);
#4400=ORIENTED_EDGE('',*,*,#3348,.F.);
#4401=ORIENTED_EDGE('',*,*,#3347,.F.);
#4402=ORIENTED_EDGE('',*,*,#3348,.T.);
#4403=ORIENTED_EDGE('',*,*,#3349,.T.);
#4404=ORIENTED_EDGE('',*,*,#3350,.T.);
#4405=ORIENTED_EDGE('',*,*,#3351,.T.);
#4406=ORIENTED_EDGE('',*,*,#3352,.F.);
#4407=ORIENTED_EDGE('',*,*,#3353,.F.);
#4408=ORIENTED_EDGE('',*,*,#3354,.T.);
#4409=ORIENTED_EDGE('',*,*,#3355,.T.);
#4410=ORIENTED_EDGE('',*,*,#3356,.T.);
#4411=ORIENTED_EDGE('',*,*,#3354,.F.);
#4412=ORIENTED_EDGE('',*,*,#3357,.F.);
#4413=ORIENTED_EDGE('',*,*,#3351,.F.);
#4414=ORIENTED_EDGE('',*,*,#3358,.T.);
#4415=ORIENTED_EDGE('',*,*,#3359,.T.);
#4416=ORIENTED_EDGE('',*,*,#3360,.T.);
#4417=ORIENTED_EDGE('',*,*,#3361,.T.);
#4418=ORIENTED_EDGE('',*,*,#3362,.T.);
#4419=ORIENTED_EDGE('',*,*,#3363,.T.);
#4420=ORIENTED_EDGE('',*,*,#3364,.T.);
#4421=ORIENTED_EDGE('',*,*,#3365,.T.);
#4422=ORIENTED_EDGE('',*,*,#3366,.T.);
#4423=ORIENTED_EDGE('',*,*,#3367,.T.);
#4424=ORIENTED_EDGE('',*,*,#3368,.T.);
#4425=ORIENTED_EDGE('',*,*,#3369,.T.);
#4426=ORIENTED_EDGE('',*,*,#3370,.T.);
#4427=ORIENTED_EDGE('',*,*,#3371,.T.);
#4428=ORIENTED_EDGE('',*,*,#3372,.T.);
#4429=ORIENTED_EDGE('',*,*,#3373,.T.);
#4430=ORIENTED_EDGE('',*,*,#3374,.F.);
#4431=ORIENTED_EDGE('',*,*,#3375,.F.);
#4432=ORIENTED_EDGE('',*,*,#3376,.F.);
#4433=ORIENTED_EDGE('',*,*,#3377,.T.);
#4434=ORIENTED_EDGE('',*,*,#3378,.F.);
#4435=ORIENTED_EDGE('',*,*,#3379,.T.);
#4436=ORIENTED_EDGE('',*,*,#3380,.T.);
#4437=ORIENTED_EDGE('',*,*,#3374,.T.);
#4438=ORIENTED_EDGE('',*,*,#3375,.T.);
#4439=ORIENTED_EDGE('',*,*,#3376,.T.);
#4440=ORIENTED_EDGE('',*,*,#3352,.T.);
#4441=ORIENTED_EDGE('',*,*,#3357,.T.);
#4442=ORIENTED_EDGE('',*,*,#3353,.T.);
#4443=ORIENTED_EDGE('',*,*,#3381,.F.);
#4444=ORIENTED_EDGE('',*,*,#3382,.T.);
#4445=ORIENTED_EDGE('',*,*,#3383,.T.);
#4446=ORIENTED_EDGE('',*,*,#3384,.T.);
#4447=ORIENTED_EDGE('',*,*,#3385,.T.);
#4448=ORIENTED_EDGE('',*,*,#3386,.T.);
#4449=ORIENTED_EDGE('',*,*,#3387,.T.);
#4450=ORIENTED_EDGE('',*,*,#3388,.T.);
#4451=ORIENTED_EDGE('',*,*,#3381,.T.);
#4452=ORIENTED_EDGE('',*,*,#3389,.T.);
#4453=ORIENTED_EDGE('',*,*,#3385,.F.);
#4454=ORIENTED_EDGE('',*,*,#3390,.T.);
#4455=ORIENTED_EDGE('',*,*,#3391,.F.);
#4456=ORIENTED_EDGE('',*,*,#3372,.F.);
#4457=ORIENTED_EDGE('',*,*,#3392,.F.);
#4458=ORIENTED_EDGE('',*,*,#3387,.F.);
#4459=ORIENTED_EDGE('',*,*,#3392,.T.);
#4460=ORIENTED_EDGE('',*,*,#3371,.F.);
#4461=ORIENTED_EDGE('',*,*,#3393,.F.);
#4462=ORIENTED_EDGE('',*,*,#3382,.F.);
#4463=ORIENTED_EDGE('',*,*,#3389,.F.);
#4464=ORIENTED_EDGE('',*,*,#3388,.F.);
#4465=ORIENTED_EDGE('',*,*,#3390,.F.);
#4466=ORIENTED_EDGE('',*,*,#3384,.F.);
#4467=ORIENTED_EDGE('',*,*,#3394,.F.);
#4468=ORIENTED_EDGE('',*,*,#3373,.F.);
#4469=ORIENTED_EDGE('',*,*,#3391,.T.);
#4470=ORIENTED_EDGE('',*,*,#3386,.F.);
#4471=ORIENTED_EDGE('',*,*,#3393,.T.);
#4472=ORIENTED_EDGE('',*,*,#3370,.F.);
#4473=ORIENTED_EDGE('',*,*,#3394,.T.);
#4474=ORIENTED_EDGE('',*,*,#3383,.F.);
#4475=ORIENTED_EDGE('',*,*,#3395,.F.);
#4476=ORIENTED_EDGE('',*,*,#3396,.T.);
#4477=ORIENTED_EDGE('',*,*,#3397,.T.);
#4478=ORIENTED_EDGE('',*,*,#3398,.T.);
#4479=ORIENTED_EDGE('',*,*,#3399,.T.);
#4480=ORIENTED_EDGE('',*,*,#3400,.T.);
#4481=ORIENTED_EDGE('',*,*,#3401,.T.);
#4482=ORIENTED_EDGE('',*,*,#3402,.T.);
#4483=ORIENTED_EDGE('',*,*,#3395,.T.);
#4484=ORIENTED_EDGE('',*,*,#3403,.T.);
#4485=ORIENTED_EDGE('',*,*,#3399,.F.);
#4486=ORIENTED_EDGE('',*,*,#3404,.T.);
#4487=ORIENTED_EDGE('',*,*,#3405,.F.);
#4488=ORIENTED_EDGE('',*,*,#3406,.T.);
#4489=ORIENTED_EDGE('',*,*,#3407,.T.);
#4490=ORIENTED_EDGE('',*,*,#3408,.T.);
#4491=ORIENTED_EDGE('',*,*,#3409,.T.);
#4492=ORIENTED_EDGE('',*,*,#3410,.T.);
#4493=ORIENTED_EDGE('',*,*,#3411,.T.);
#4494=ORIENTED_EDGE('',*,*,#3412,.T.);
#4495=ORIENTED_EDGE('',*,*,#3405,.T.);
#4496=ORIENTED_EDGE('',*,*,#3413,.T.);
#4497=ORIENTED_EDGE('',*,*,#3409,.F.);
#4498=ORIENTED_EDGE('',*,*,#3414,.T.);
#4499=ORIENTED_EDGE('',*,*,#3415,.F.);
#4500=ORIENTED_EDGE('',*,*,#3416,.T.);
#4501=ORIENTED_EDGE('',*,*,#3417,.T.);
#4502=ORIENTED_EDGE('',*,*,#3418,.T.);
#4503=ORIENTED_EDGE('',*,*,#3419,.T.);
#4504=ORIENTED_EDGE('',*,*,#3420,.T.);
#4505=ORIENTED_EDGE('',*,*,#3421,.T.);
#4506=ORIENTED_EDGE('',*,*,#3422,.T.);
#4507=ORIENTED_EDGE('',*,*,#3415,.T.);
#4508=ORIENTED_EDGE('',*,*,#3423,.T.);
#4509=ORIENTED_EDGE('',*,*,#3419,.F.);
#4510=ORIENTED_EDGE('',*,*,#3424,.T.);
#4511=ORIENTED_EDGE('',*,*,#3425,.F.);
#4512=ORIENTED_EDGE('',*,*,#3368,.F.);
#4513=ORIENTED_EDGE('',*,*,#3426,.F.);
#4514=ORIENTED_EDGE('',*,*,#3421,.F.);
#4515=ORIENTED_EDGE('',*,*,#3426,.T.);
#4516=ORIENTED_EDGE('',*,*,#3367,.F.);
#4517=ORIENTED_EDGE('',*,*,#3427,.F.);
#4518=ORIENTED_EDGE('',*,*,#3416,.F.);
#4519=ORIENTED_EDGE('',*,*,#3423,.F.);
#4520=ORIENTED_EDGE('',*,*,#3422,.F.);
#4521=ORIENTED_EDGE('',*,*,#3424,.F.);
#4522=ORIENTED_EDGE('',*,*,#3418,.F.);
#4523=ORIENTED_EDGE('',*,*,#3428,.F.);
#4524=ORIENTED_EDGE('',*,*,#3369,.F.);
#4525=ORIENTED_EDGE('',*,*,#3425,.T.);
#4526=ORIENTED_EDGE('',*,*,#3420,.F.);
#4527=ORIENTED_EDGE('',*,*,#3427,.T.);
#4528=ORIENTED_EDGE('',*,*,#3366,.F.);
#4529=ORIENTED_EDGE('',*,*,#3428,.T.);
#4530=ORIENTED_EDGE('',*,*,#3417,.F.);
#4531=ORIENTED_EDGE('',*,*,#3429,.F.);
#4532=ORIENTED_EDGE('',*,*,#3364,.F.);
#4533=ORIENTED_EDGE('',*,*,#3430,.F.);
#4534=ORIENTED_EDGE('',*,*,#3411,.F.);
#4535=ORIENTED_EDGE('',*,*,#3430,.T.);
#4536=ORIENTED_EDGE('',*,*,#3363,.F.);
#4537=ORIENTED_EDGE('',*,*,#3431,.F.);
#4538=ORIENTED_EDGE('',*,*,#3406,.F.);
#4539=ORIENTED_EDGE('',*,*,#3413,.F.);
#4540=ORIENTED_EDGE('',*,*,#3412,.F.);
#4541=ORIENTED_EDGE('',*,*,#3414,.F.);
#4542=ORIENTED_EDGE('',*,*,#3408,.F.);
#4543=ORIENTED_EDGE('',*,*,#3432,.F.);
#4544=ORIENTED_EDGE('',*,*,#3365,.F.);
#4545=ORIENTED_EDGE('',*,*,#3429,.T.);
#4546=ORIENTED_EDGE('',*,*,#3410,.F.);
#4547=ORIENTED_EDGE('',*,*,#3431,.T.);
#4548=ORIENTED_EDGE('',*,*,#3362,.F.);
#4549=ORIENTED_EDGE('',*,*,#3432,.T.);
#4550=ORIENTED_EDGE('',*,*,#3407,.F.);
#4551=ORIENTED_EDGE('',*,*,#3433,.F.);
#4552=ORIENTED_EDGE('',*,*,#3360,.F.);
#4553=ORIENTED_EDGE('',*,*,#3434,.F.);
#4554=ORIENTED_EDGE('',*,*,#3401,.F.);
#4555=ORIENTED_EDGE('',*,*,#3434,.T.);
#4556=ORIENTED_EDGE('',*,*,#3359,.F.);
#4557=ORIENTED_EDGE('',*,*,#3435,.F.);
#4558=ORIENTED_EDGE('',*,*,#3396,.F.);
#4559=ORIENTED_EDGE('',*,*,#3403,.F.);
#4560=ORIENTED_EDGE('',*,*,#3402,.F.);
#4561=ORIENTED_EDGE('',*,*,#3404,.F.);
#4562=ORIENTED_EDGE('',*,*,#3398,.F.);
#4563=ORIENTED_EDGE('',*,*,#3436,.F.);
#4564=ORIENTED_EDGE('',*,*,#3361,.F.);
#4565=ORIENTED_EDGE('',*,*,#3433,.T.);
#4566=ORIENTED_EDGE('',*,*,#3400,.F.);
#4567=ORIENTED_EDGE('',*,*,#3435,.T.);
#4568=ORIENTED_EDGE('',*,*,#3358,.F.);
#4569=ORIENTED_EDGE('',*,*,#3436,.T.);
#4570=ORIENTED_EDGE('',*,*,#3397,.F.);
#4571=ORIENTED_EDGE('',*,*,#3349,.F.);
#4572=ORIENTED_EDGE('',*,*,#3350,.F.);
#4573=ORIENTED_EDGE('',*,*,#3437,.T.);
#4574=ORIENTED_EDGE('',*,*,#3379,.F.);
#4575=ORIENTED_EDGE('',*,*,#3437,.F.);
#4576=ORIENTED_EDGE('',*,*,#3377,.F.);
#4577=ORIENTED_EDGE('',*,*,#3438,.T.);
#4578=ORIENTED_EDGE('',*,*,#3355,.F.);
#4579=ORIENTED_EDGE('',*,*,#3356,.F.);
#4580=ORIENTED_EDGE('',*,*,#3438,.F.);
#4581=ORIENTED_EDGE('',*,*,#3380,.F.);
#4582=ORIENTED_EDGE('',*,*,#3439,.T.);
#4583=ORIENTED_EDGE('',*,*,#3378,.T.);
#4584=ORIENTED_EDGE('',*,*,#3439,.F.);
#4585=ORIENTED_EDGE('',*,*,#3440,.T.);
#4586=ORIENTED_EDGE('',*,*,#3441,.T.);
#4587=ORIENTED_EDGE('',*,*,#3442,.T.);
#4588=ORIENTED_EDGE('',*,*,#3443,.T.);
#4589=ORIENTED_EDGE('',*,*,#3444,.F.);
#4590=ORIENTED_EDGE('',*,*,#3445,.T.);
#4591=ORIENTED_EDGE('',*,*,#3441,.F.);
#4592=ORIENTED_EDGE('',*,*,#3446,.F.);
#4593=ORIENTED_EDGE('',*,*,#3447,.F.);
#4594=ORIENTED_EDGE('',*,*,#3448,.T.);
#4595=ORIENTED_EDGE('',*,*,#3442,.F.);
#4596=ORIENTED_EDGE('',*,*,#3445,.F.);
#4597=ORIENTED_EDGE('',*,*,#3449,.F.);
#4598=ORIENTED_EDGE('',*,*,#3450,.T.);
#4599=ORIENTED_EDGE('',*,*,#3443,.F.);
#4600=ORIENTED_EDGE('',*,*,#3448,.F.);
#4601=ORIENTED_EDGE('',*,*,#3450,.F.);
#4602=ORIENTED_EDGE('',*,*,#3451,.F.);
#4603=ORIENTED_EDGE('',*,*,#3446,.T.);
#4604=ORIENTED_EDGE('',*,*,#3440,.F.);
#4605=ORIENTED_EDGE('',*,*,#3449,.T.);
#4606=ORIENTED_EDGE('',*,*,#3447,.T.);
#4607=ORIENTED_EDGE('',*,*,#3444,.T.);
#4608=ORIENTED_EDGE('',*,*,#3451,.T.);
#4609=ORIENTED_EDGE('',*,*,#3452,.T.);
#4610=ORIENTED_EDGE('',*,*,#3453,.T.);
#4611=ORIENTED_EDGE('',*,*,#3454,.T.);
#4612=ORIENTED_EDGE('',*,*,#3455,.T.);
#4613=ORIENTED_EDGE('',*,*,#3456,.F.);
#4614=ORIENTED_EDGE('',*,*,#3457,.T.);
#4615=ORIENTED_EDGE('',*,*,#3453,.F.);
#4616=ORIENTED_EDGE('',*,*,#3458,.F.);
#4617=ORIENTED_EDGE('',*,*,#3459,.F.);
#4618=ORIENTED_EDGE('',*,*,#3460,.T.);
#4619=ORIENTED_EDGE('',*,*,#3454,.F.);
#4620=ORIENTED_EDGE('',*,*,#3457,.F.);
#4621=ORIENTED_EDGE('',*,*,#3461,.F.);
#4622=ORIENTED_EDGE('',*,*,#3462,.T.);
#4623=ORIENTED_EDGE('',*,*,#3455,.F.);
#4624=ORIENTED_EDGE('',*,*,#3460,.F.);
#4625=ORIENTED_EDGE('',*,*,#3452,.F.);
#4626=ORIENTED_EDGE('',*,*,#3462,.F.);
#4627=ORIENTED_EDGE('',*,*,#3463,.F.);
#4628=ORIENTED_EDGE('',*,*,#3458,.T.);
#4629=ORIENTED_EDGE('',*,*,#3461,.T.);
#4630=ORIENTED_EDGE('',*,*,#3459,.T.);
#4631=ORIENTED_EDGE('',*,*,#3456,.T.);
#4632=ORIENTED_EDGE('',*,*,#3463,.T.);
#4633=ORIENTED_EDGE('',*,*,#3464,.T.);
#4634=ORIENTED_EDGE('',*,*,#3465,.T.);
#4635=ORIENTED_EDGE('',*,*,#3466,.T.);
#4636=ORIENTED_EDGE('',*,*,#3467,.T.);
#4637=ORIENTED_EDGE('',*,*,#3468,.F.);
#4638=ORIENTED_EDGE('',*,*,#3469,.T.);
#4639=ORIENTED_EDGE('',*,*,#3465,.F.);
#4640=ORIENTED_EDGE('',*,*,#3470,.F.);
#4641=ORIENTED_EDGE('',*,*,#3471,.F.);
#4642=ORIENTED_EDGE('',*,*,#3472,.T.);
#4643=ORIENTED_EDGE('',*,*,#3466,.F.);
#4644=ORIENTED_EDGE('',*,*,#3469,.F.);
#4645=ORIENTED_EDGE('',*,*,#3473,.F.);
#4646=ORIENTED_EDGE('',*,*,#3474,.T.);
#4647=ORIENTED_EDGE('',*,*,#3467,.F.);
#4648=ORIENTED_EDGE('',*,*,#3472,.F.);
#4649=ORIENTED_EDGE('',*,*,#3474,.F.);
#4650=ORIENTED_EDGE('',*,*,#3475,.F.);
#4651=ORIENTED_EDGE('',*,*,#3470,.T.);
#4652=ORIENTED_EDGE('',*,*,#3464,.F.);
#4653=ORIENTED_EDGE('',*,*,#3473,.T.);
#4654=ORIENTED_EDGE('',*,*,#3471,.T.);
#4655=ORIENTED_EDGE('',*,*,#3468,.T.);
#4656=ORIENTED_EDGE('',*,*,#3475,.T.);
#4657=ORIENTED_EDGE('',*,*,#3476,.F.);
#4658=ORIENTED_EDGE('',*,*,#3477,.F.);
#4659=ORIENTED_EDGE('',*,*,#3478,.F.);
#4660=ORIENTED_EDGE('',*,*,#3479,.T.);
#4661=ORIENTED_EDGE('',*,*,#3480,.F.);
#4662=ORIENTED_EDGE('',*,*,#3481,.T.);
#4663=ORIENTED_EDGE('',*,*,#3482,.F.);
#4664=ORIENTED_EDGE('',*,*,#3483,.F.);
#4665=ORIENTED_EDGE('',*,*,#3484,.F.);
#4666=ORIENTED_EDGE('',*,*,#3485,.T.);
#4667=ORIENTED_EDGE('',*,*,#3486,.F.);
#4668=ORIENTED_EDGE('',*,*,#3487,.F.);
#4669=ORIENTED_EDGE('',*,*,#3477,.T.);
#4670=ORIENTED_EDGE('',*,*,#3488,.T.);
#4671=ORIENTED_EDGE('',*,*,#3489,.F.);
#4672=ORIENTED_EDGE('',*,*,#3490,.T.);
#4673=ORIENTED_EDGE('',*,*,#3483,.T.);
#4674=ORIENTED_EDGE('',*,*,#3491,.T.);
#4675=ORIENTED_EDGE('',*,*,#3492,.F.);
#4676=ORIENTED_EDGE('',*,*,#3493,.T.);
#4677=ORIENTED_EDGE('',*,*,#3487,.T.);
#4678=ORIENTED_EDGE('',*,*,#3494,.T.);
#4679=ORIENTED_EDGE('',*,*,#3495,.F.);
#4680=ORIENTED_EDGE('',*,*,#3496,.T.);
#4681=ORIENTED_EDGE('',*,*,#3497,.T.);
#4682=ORIENTED_EDGE('',*,*,#3498,.F.);
#4683=ORIENTED_EDGE('',*,*,#3499,.F.);
#4684=ORIENTED_EDGE('',*,*,#3500,.F.);
#4685=ORIENTED_EDGE('',*,*,#3501,.T.);
#4686=ORIENTED_EDGE('',*,*,#3502,.F.);
#4687=ORIENTED_EDGE('',*,*,#3503,.T.);
#4688=ORIENTED_EDGE('',*,*,#3504,.F.);
#4689=ORIENTED_EDGE('',*,*,#3505,.F.);
#4690=ORIENTED_EDGE('',*,*,#3506,.F.);
#4691=ORIENTED_EDGE('',*,*,#3507,.T.);
#4692=ORIENTED_EDGE('',*,*,#3508,.F.);
#4693=ORIENTED_EDGE('',*,*,#3509,.F.);
#4694=ORIENTED_EDGE('',*,*,#3499,.T.);
#4695=ORIENTED_EDGE('',*,*,#3510,.T.);
#4696=ORIENTED_EDGE('',*,*,#3511,.F.);
#4697=ORIENTED_EDGE('',*,*,#3512,.T.);
#4698=ORIENTED_EDGE('',*,*,#3505,.T.);
#4699=ORIENTED_EDGE('',*,*,#3513,.T.);
#4700=ORIENTED_EDGE('',*,*,#3514,.F.);
#4701=ORIENTED_EDGE('',*,*,#3515,.T.);
#4702=ORIENTED_EDGE('',*,*,#3509,.T.);
#4703=ORIENTED_EDGE('',*,*,#3516,.T.);
#4704=ORIENTED_EDGE('',*,*,#3517,.F.);
#4705=ORIENTED_EDGE('',*,*,#3518,.T.);
#4706=ORIENTED_EDGE('',*,*,#3519,.T.);
#4707=ORIENTED_EDGE('',*,*,#3520,.F.);
#4708=ORIENTED_EDGE('',*,*,#3521,.F.);
#4709=ORIENTED_EDGE('',*,*,#3522,.F.);
#4710=ORIENTED_EDGE('',*,*,#3523,.T.);
#4711=ORIENTED_EDGE('',*,*,#3524,.F.);
#4712=ORIENTED_EDGE('',*,*,#3525,.T.);
#4713=ORIENTED_EDGE('',*,*,#3526,.F.);
#4714=ORIENTED_EDGE('',*,*,#3527,.F.);
#4715=ORIENTED_EDGE('',*,*,#3528,.F.);
#4716=ORIENTED_EDGE('',*,*,#3529,.T.);
#4717=ORIENTED_EDGE('',*,*,#3530,.F.);
#4718=ORIENTED_EDGE('',*,*,#3531,.F.);
#4719=ORIENTED_EDGE('',*,*,#3521,.T.);
#4720=ORIENTED_EDGE('',*,*,#3532,.T.);
#4721=ORIENTED_EDGE('',*,*,#3533,.F.);
#4722=ORIENTED_EDGE('',*,*,#3534,.T.);
#4723=ORIENTED_EDGE('',*,*,#3527,.T.);
#4724=ORIENTED_EDGE('',*,*,#3535,.T.);
#4725=ORIENTED_EDGE('',*,*,#3536,.F.);
#4726=ORIENTED_EDGE('',*,*,#3537,.T.);
#4727=ORIENTED_EDGE('',*,*,#3531,.T.);
#4728=ORIENTED_EDGE('',*,*,#3538,.T.);
#4729=ORIENTED_EDGE('',*,*,#3539,.F.);
#4730=ORIENTED_EDGE('',*,*,#3540,.T.);
#4731=ORIENTED_EDGE('',*,*,#3541,.T.);
#4732=ORIENTED_EDGE('',*,*,#3542,.T.);
#4733=ORIENTED_EDGE('',*,*,#3543,.T.);
#4734=ORIENTED_EDGE('',*,*,#3544,.F.);
#4735=ORIENTED_EDGE('',*,*,#3545,.F.);
#4736=ORIENTED_EDGE('',*,*,#3546,.T.);
#4737=ORIENTED_EDGE('',*,*,#3547,.F.);
#4738=ORIENTED_EDGE('',*,*,#3546,.F.);
#4739=ORIENTED_EDGE('',*,*,#3548,.F.);
#4740=ORIENTED_EDGE('',*,*,#3549,.F.);
#4741=ORIENTED_EDGE('',*,*,#3543,.F.);
#4742=ORIENTED_EDGE('',*,*,#3550,.F.);
#4743=ORIENTED_EDGE('',*,*,#3551,.F.);
#4744=ORIENTED_EDGE('',*,*,#3552,.F.);
#4745=ORIENTED_EDGE('',*,*,#3553,.F.);
#4746=ORIENTED_EDGE('',*,*,#3547,.T.);
#4747=ORIENTED_EDGE('',*,*,#3554,.F.);
#4748=ORIENTED_EDGE('',*,*,#3542,.F.);
#4749=ORIENTED_EDGE('',*,*,#3555,.F.);
#4750=ORIENTED_EDGE('',*,*,#3556,.F.);
#4751=ORIENTED_EDGE('',*,*,#3557,.T.);
#4752=ORIENTED_EDGE('',*,*,#3554,.T.);
#4753=ORIENTED_EDGE('',*,*,#3557,.F.);
#4754=ORIENTED_EDGE('',*,*,#3556,.T.);
#4755=ORIENTED_EDGE('',*,*,#3558,.F.);
#4756=ORIENTED_EDGE('',*,*,#3559,.T.);
#4757=ORIENTED_EDGE('',*,*,#3544,.T.);
#4758=ORIENTED_EDGE('',*,*,#3549,.T.);
#4759=ORIENTED_EDGE('',*,*,#3548,.T.);
#4760=ORIENTED_EDGE('',*,*,#3545,.T.);
#4761=ORIENTED_EDGE('',*,*,#3559,.F.);
#4762=ORIENTED_EDGE('',*,*,#3560,.T.);
#4763=ORIENTED_EDGE('',*,*,#3525,.F.);
#4764=ORIENTED_EDGE('',*,*,#3561,.F.);
#4765=ORIENTED_EDGE('',*,*,#3562,.T.);
#4766=ORIENTED_EDGE('',*,*,#3563,.T.);
#4767=ORIENTED_EDGE('',*,*,#3523,.F.);
#4768=ORIENTED_EDGE('',*,*,#3564,.F.);
#4769=ORIENTED_EDGE('',*,*,#3565,.T.);
#4770=ORIENTED_EDGE('',*,*,#3566,.T.);
#4771=ORIENTED_EDGE('',*,*,#3529,.F.);
#4772=ORIENTED_EDGE('',*,*,#3567,.F.);
#4773=ORIENTED_EDGE('',*,*,#3568,.T.);
#4774=ORIENTED_EDGE('',*,*,#3569,.T.);
#4775=ORIENTED_EDGE('',*,*,#3570,.T.);
#4776=ORIENTED_EDGE('',*,*,#3571,.T.);
#4777=ORIENTED_EDGE('',*,*,#3572,.T.);
#4778=ORIENTED_EDGE('',*,*,#3560,.F.);
#4779=ORIENTED_EDGE('',*,*,#3572,.F.);
#4780=ORIENTED_EDGE('',*,*,#3573,.F.);
#4781=ORIENTED_EDGE('',*,*,#3574,.F.);
#4782=ORIENTED_EDGE('',*,*,#3575,.F.);
#4783=ORIENTED_EDGE('',*,*,#3576,.T.);
#4784=ORIENTED_EDGE('',*,*,#3541,.F.);
#4785=ORIENTED_EDGE('',*,*,#3576,.F.);
#4786=ORIENTED_EDGE('',*,*,#3577,.F.);
#4787=ORIENTED_EDGE('',*,*,#3570,.F.);
#4788=ORIENTED_EDGE('',*,*,#3571,.F.);
#4789=ORIENTED_EDGE('',*,*,#3578,.T.);
#4790=ORIENTED_EDGE('',*,*,#3558,.T.);
#4791=ORIENTED_EDGE('',*,*,#3578,.F.);
#4792=ORIENTED_EDGE('',*,*,#3579,.F.);
#4793=ORIENTED_EDGE('',*,*,#3580,.T.);
#4794=ORIENTED_EDGE('',*,*,#3553,.T.);
#4795=ORIENTED_EDGE('',*,*,#3552,.T.);
#4796=ORIENTED_EDGE('',*,*,#3580,.F.);
#4797=ORIENTED_EDGE('',*,*,#3581,.F.);
#4798=ORIENTED_EDGE('',*,*,#3582,.T.);
#4799=ORIENTED_EDGE('',*,*,#3551,.T.);
#4800=ORIENTED_EDGE('',*,*,#3550,.T.);
#4801=ORIENTED_EDGE('',*,*,#3582,.F.);
#4802=ORIENTED_EDGE('',*,*,#3583,.T.);
#4803=ORIENTED_EDGE('',*,*,#3584,.T.);
#4804=ORIENTED_EDGE('',*,*,#3479,.F.);
#4805=ORIENTED_EDGE('',*,*,#3585,.F.);
#4806=ORIENTED_EDGE('',*,*,#3586,.T.);
#4807=ORIENTED_EDGE('',*,*,#3587,.T.);
#4808=ORIENTED_EDGE('',*,*,#3485,.F.);
#4809=ORIENTED_EDGE('',*,*,#3588,.F.);
#4810=ORIENTED_EDGE('',*,*,#3589,.T.);
#4811=ORIENTED_EDGE('',*,*,#3590,.T.);
#4812=ORIENTED_EDGE('',*,*,#3481,.F.);
#4813=ORIENTED_EDGE('',*,*,#3591,.F.);
#4814=ORIENTED_EDGE('',*,*,#3592,.T.);
#4815=ORIENTED_EDGE('',*,*,#3593,.T.);
#4816=ORIENTED_EDGE('',*,*,#3594,.T.);
#4817=ORIENTED_EDGE('',*,*,#3595,.T.);
#4818=ORIENTED_EDGE('',*,*,#3583,.F.);
#4819=ORIENTED_EDGE('',*,*,#3595,.F.);
#4820=ORIENTED_EDGE('',*,*,#3596,.T.);
#4821=ORIENTED_EDGE('',*,*,#3597,.T.);
#4822=ORIENTED_EDGE('',*,*,#3501,.F.);
#4823=ORIENTED_EDGE('',*,*,#3598,.F.);
#4824=ORIENTED_EDGE('',*,*,#3599,.T.);
#4825=ORIENTED_EDGE('',*,*,#3600,.T.);
#4826=ORIENTED_EDGE('',*,*,#3507,.F.);
#4827=ORIENTED_EDGE('',*,*,#3601,.F.);
#4828=ORIENTED_EDGE('',*,*,#3602,.T.);
#4829=ORIENTED_EDGE('',*,*,#3603,.T.);
#4830=ORIENTED_EDGE('',*,*,#3503,.F.);
#4831=ORIENTED_EDGE('',*,*,#3604,.F.);
#4832=ORIENTED_EDGE('',*,*,#3605,.T.);
#4833=ORIENTED_EDGE('',*,*,#3606,.T.);
#4834=ORIENTED_EDGE('',*,*,#3607,.T.);
#4835=ORIENTED_EDGE('',*,*,#3608,.T.);
#4836=ORIENTED_EDGE('',*,*,#3596,.F.);
#4837=ORIENTED_EDGE('',*,*,#3608,.F.);
#4838=ORIENTED_EDGE('',*,*,#3609,.F.);
#4839=ORIENTED_EDGE('',*,*,#3610,.F.);
#4840=ORIENTED_EDGE('',*,*,#3611,.T.);
#4841=ORIENTED_EDGE('',*,*,#3497,.F.);
#4842=ORIENTED_EDGE('',*,*,#3611,.F.);
#4843=ORIENTED_EDGE('',*,*,#3612,.F.);
#4844=ORIENTED_EDGE('',*,*,#3613,.F.);
#4845=ORIENTED_EDGE('',*,*,#3614,.T.);
#4846=ORIENTED_EDGE('',*,*,#3519,.F.);
#4847=ORIENTED_EDGE('',*,*,#3614,.F.);
#4848=ORIENTED_EDGE('',*,*,#3606,.F.);
#4849=ORIENTED_EDGE('',*,*,#3607,.F.);
#4850=ORIENTED_EDGE('',*,*,#3615,.T.);
#4851=ORIENTED_EDGE('',*,*,#3579,.T.);
#4852=ORIENTED_EDGE('',*,*,#3615,.F.);
#4853=ORIENTED_EDGE('',*,*,#3593,.F.);
#4854=ORIENTED_EDGE('',*,*,#3594,.F.);
#4855=ORIENTED_EDGE('',*,*,#3616,.T.);
#4856=ORIENTED_EDGE('',*,*,#3581,.T.);
#4857=ORIENTED_EDGE('',*,*,#3616,.F.);
#4858=ORIENTED_EDGE('',*,*,#3617,.T.);
#4859=ORIENTED_EDGE('',*,*,#3617,.F.);
#4860=ORIENTED_EDGE('',*,*,#3618,.T.);
#4861=ORIENTED_EDGE('',*,*,#3577,.T.);
#4862=ORIENTED_EDGE('',*,*,#3575,.T.);
#4863=ORIENTED_EDGE('',*,*,#3619,.T.);
#4864=ORIENTED_EDGE('',*,*,#3555,.T.);
#4865=ORIENTED_EDGE('',*,*,#3619,.F.);
#4866=ORIENTED_EDGE('',*,*,#3574,.T.);
#4867=ORIENTED_EDGE('',*,*,#3573,.T.);
#4868=ORIENTED_EDGE('',*,*,#3618,.F.);
#4869=ORIENTED_EDGE('',*,*,#3612,.T.);
#4870=ORIENTED_EDGE('',*,*,#3613,.T.);
#4871=ORIENTED_EDGE('',*,*,#3609,.T.);
#4872=ORIENTED_EDGE('',*,*,#3610,.T.);
#4873=ORIENTED_EDGE('',*,*,#3530,.T.);
#4874=ORIENTED_EDGE('',*,*,#3566,.F.);
#4875=ORIENTED_EDGE('',*,*,#3620,.T.);
#4876=ORIENTED_EDGE('',*,*,#3538,.F.);
#4877=ORIENTED_EDGE('',*,*,#3522,.T.);
#4878=ORIENTED_EDGE('',*,*,#3540,.F.);
#4879=ORIENTED_EDGE('',*,*,#3621,.T.);
#4880=ORIENTED_EDGE('',*,*,#3564,.T.);
#4881=ORIENTED_EDGE('',*,*,#3539,.T.);
#4882=ORIENTED_EDGE('',*,*,#3620,.F.);
#4883=ORIENTED_EDGE('',*,*,#3565,.F.);
#4884=ORIENTED_EDGE('',*,*,#3621,.F.);
#4885=ORIENTED_EDGE('',*,*,#3526,.T.);
#4886=ORIENTED_EDGE('',*,*,#3569,.F.);
#4887=ORIENTED_EDGE('',*,*,#3622,.T.);
#4888=ORIENTED_EDGE('',*,*,#3535,.F.);
#4889=ORIENTED_EDGE('',*,*,#3528,.T.);
#4890=ORIENTED_EDGE('',*,*,#3537,.F.);
#4891=ORIENTED_EDGE('',*,*,#3623,.T.);
#4892=ORIENTED_EDGE('',*,*,#3567,.T.);
#4893=ORIENTED_EDGE('',*,*,#3536,.T.);
#4894=ORIENTED_EDGE('',*,*,#3622,.F.);
#4895=ORIENTED_EDGE('',*,*,#3568,.F.);
#4896=ORIENTED_EDGE('',*,*,#3623,.F.);
#4897=ORIENTED_EDGE('',*,*,#3520,.T.);
#4898=ORIENTED_EDGE('',*,*,#3563,.F.);
#4899=ORIENTED_EDGE('',*,*,#3624,.T.);
#4900=ORIENTED_EDGE('',*,*,#3532,.F.);
#4901=ORIENTED_EDGE('',*,*,#3524,.T.);
#4902=ORIENTED_EDGE('',*,*,#3534,.F.);
#4903=ORIENTED_EDGE('',*,*,#3625,.T.);
#4904=ORIENTED_EDGE('',*,*,#3561,.T.);
#4905=ORIENTED_EDGE('',*,*,#3533,.T.);
#4906=ORIENTED_EDGE('',*,*,#3624,.F.);
#4907=ORIENTED_EDGE('',*,*,#3562,.F.);
#4908=ORIENTED_EDGE('',*,*,#3625,.F.);
#4909=ORIENTED_EDGE('',*,*,#3508,.T.);
#4910=ORIENTED_EDGE('',*,*,#3600,.F.);
#4911=ORIENTED_EDGE('',*,*,#3626,.T.);
#4912=ORIENTED_EDGE('',*,*,#3516,.F.);
#4913=ORIENTED_EDGE('',*,*,#3500,.T.);
#4914=ORIENTED_EDGE('',*,*,#3518,.F.);
#4915=ORIENTED_EDGE('',*,*,#3627,.T.);
#4916=ORIENTED_EDGE('',*,*,#3598,.T.);
#4917=ORIENTED_EDGE('',*,*,#3517,.T.);
#4918=ORIENTED_EDGE('',*,*,#3626,.F.);
#4919=ORIENTED_EDGE('',*,*,#3599,.F.);
#4920=ORIENTED_EDGE('',*,*,#3627,.F.);
#4921=ORIENTED_EDGE('',*,*,#3504,.T.);
#4922=ORIENTED_EDGE('',*,*,#3603,.F.);
#4923=ORIENTED_EDGE('',*,*,#3628,.T.);
#4924=ORIENTED_EDGE('',*,*,#3513,.F.);
#4925=ORIENTED_EDGE('',*,*,#3506,.T.);
#4926=ORIENTED_EDGE('',*,*,#3515,.F.);
#4927=ORIENTED_EDGE('',*,*,#3629,.T.);
#4928=ORIENTED_EDGE('',*,*,#3601,.T.);
#4929=ORIENTED_EDGE('',*,*,#3514,.T.);
#4930=ORIENTED_EDGE('',*,*,#3628,.F.);
#4931=ORIENTED_EDGE('',*,*,#3602,.F.);
#4932=ORIENTED_EDGE('',*,*,#3629,.F.);
#4933=ORIENTED_EDGE('',*,*,#3498,.T.);
#4934=ORIENTED_EDGE('',*,*,#3597,.F.);
#4935=ORIENTED_EDGE('',*,*,#3630,.T.);
#4936=ORIENTED_EDGE('',*,*,#3510,.F.);
#4937=ORIENTED_EDGE('',*,*,#3502,.T.);
#4938=ORIENTED_EDGE('',*,*,#3512,.F.);
#4939=ORIENTED_EDGE('',*,*,#3631,.T.);
#4940=ORIENTED_EDGE('',*,*,#3604,.T.);
#4941=ORIENTED_EDGE('',*,*,#3511,.T.);
#4942=ORIENTED_EDGE('',*,*,#3630,.F.);
#4943=ORIENTED_EDGE('',*,*,#3605,.F.);
#4944=ORIENTED_EDGE('',*,*,#3631,.F.);
#4945=ORIENTED_EDGE('',*,*,#3486,.T.);
#4946=ORIENTED_EDGE('',*,*,#3587,.F.);
#4947=ORIENTED_EDGE('',*,*,#3632,.T.);
#4948=ORIENTED_EDGE('',*,*,#3494,.F.);
#4949=ORIENTED_EDGE('',*,*,#3478,.T.);
#4950=ORIENTED_EDGE('',*,*,#3496,.F.);
#4951=ORIENTED_EDGE('',*,*,#3633,.T.);
#4952=ORIENTED_EDGE('',*,*,#3585,.T.);
#4953=ORIENTED_EDGE('',*,*,#3495,.T.);
#4954=ORIENTED_EDGE('',*,*,#3632,.F.);
#4955=ORIENTED_EDGE('',*,*,#3586,.F.);
#4956=ORIENTED_EDGE('',*,*,#3633,.F.);
#4957=ORIENTED_EDGE('',*,*,#3482,.T.);
#4958=ORIENTED_EDGE('',*,*,#3590,.F.);
#4959=ORIENTED_EDGE('',*,*,#3634,.T.);
#4960=ORIENTED_EDGE('',*,*,#3491,.F.);
#4961=ORIENTED_EDGE('',*,*,#3484,.T.);
#4962=ORIENTED_EDGE('',*,*,#3493,.F.);
#4963=ORIENTED_EDGE('',*,*,#3635,.T.);
#4964=ORIENTED_EDGE('',*,*,#3588,.T.);
#4965=ORIENTED_EDGE('',*,*,#3492,.T.);
#4966=ORIENTED_EDGE('',*,*,#3634,.F.);
#4967=ORIENTED_EDGE('',*,*,#3589,.F.);
#4968=ORIENTED_EDGE('',*,*,#3635,.F.);
#4969=ORIENTED_EDGE('',*,*,#3476,.T.);
#4970=ORIENTED_EDGE('',*,*,#3584,.F.);
#4971=ORIENTED_EDGE('',*,*,#3636,.T.);
#4972=ORIENTED_EDGE('',*,*,#3488,.F.);
#4973=ORIENTED_EDGE('',*,*,#3480,.T.);
#4974=ORIENTED_EDGE('',*,*,#3490,.F.);
#4975=ORIENTED_EDGE('',*,*,#3637,.T.);
#4976=ORIENTED_EDGE('',*,*,#3591,.T.);
#4977=ORIENTED_EDGE('',*,*,#3489,.T.);
#4978=ORIENTED_EDGE('',*,*,#3636,.F.);
#4979=ORIENTED_EDGE('',*,*,#3592,.F.);
#4980=ORIENTED_EDGE('',*,*,#3637,.F.);
#4981=ORIENTED_EDGE('',*,*,#3638,.T.);
#4982=ORIENTED_EDGE('',*,*,#3639,.T.);
#4983=ORIENTED_EDGE('',*,*,#3640,.F.);
#4984=ORIENTED_EDGE('',*,*,#3639,.F.);
#4985=ORIENTED_EDGE('',*,*,#3640,.T.);
#4986=ORIENTED_EDGE('',*,*,#3641,.F.);
#4987=ORIENTED_EDGE('',*,*,#3638,.F.);
#4988=ORIENTED_EDGE('',*,*,#3642,.F.);
#4989=ORIENTED_EDGE('',*,*,#3643,.T.);
#4990=ORIENTED_EDGE('',*,*,#3644,.T.);
#4991=ORIENTED_EDGE('',*,*,#3645,.T.);
#4992=ORIENTED_EDGE('',*,*,#3644,.F.);
#4993=ORIENTED_EDGE('',*,*,#3645,.F.);
#4994=ORIENTED_EDGE('',*,*,#3646,.T.);
#4995=ORIENTED_EDGE('',*,*,#3642,.T.);
#4996=ORIENTED_EDGE('',*,*,#3646,.F.);
#4997=ORIENTED_EDGE('',*,*,#3647,.T.);
#4998=ORIENTED_EDGE('',*,*,#3643,.F.);
#4999=ORIENTED_EDGE('',*,*,#3641,.T.);
#5000=ORIENTED_EDGE('',*,*,#3648,.T.);
#5001=ORIENTED_EDGE('',*,*,#3647,.F.);
#5002=ORIENTED_EDGE('',*,*,#3648,.F.);
#5003=ORIENTED_EDGE('',*,*,#3649,.T.);
#5004=ORIENTED_EDGE('',*,*,#3650,.T.);
#5005=ORIENTED_EDGE('',*,*,#3651,.F.);
#5006=ORIENTED_EDGE('',*,*,#3650,.F.);
#5007=ORIENTED_EDGE('',*,*,#3651,.T.);
#5008=ORIENTED_EDGE('',*,*,#3652,.F.);
#5009=ORIENTED_EDGE('',*,*,#3649,.F.);
#5010=ORIENTED_EDGE('',*,*,#3653,.F.);
#5011=ORIENTED_EDGE('',*,*,#3654,.T.);
#5012=ORIENTED_EDGE('',*,*,#3655,.T.);
#5013=ORIENTED_EDGE('',*,*,#3656,.T.);
#5014=ORIENTED_EDGE('',*,*,#3655,.F.);
#5015=ORIENTED_EDGE('',*,*,#3656,.F.);
#5016=ORIENTED_EDGE('',*,*,#3657,.T.);
#5017=ORIENTED_EDGE('',*,*,#3653,.T.);
#5018=ORIENTED_EDGE('',*,*,#3657,.F.);
#5019=ORIENTED_EDGE('',*,*,#3658,.T.);
#5020=ORIENTED_EDGE('',*,*,#3654,.F.);
#5021=ORIENTED_EDGE('',*,*,#3652,.T.);
#5022=ORIENTED_EDGE('',*,*,#3659,.T.);
#5023=ORIENTED_EDGE('',*,*,#3658,.F.);
#5024=ORIENTED_EDGE('',*,*,#3659,.F.);
#5025=ORIENTED_EDGE('',*,*,#3660,.T.);
#5026=ORIENTED_EDGE('',*,*,#3661,.T.);
#5027=ORIENTED_EDGE('',*,*,#3662,.F.);
#5028=ORIENTED_EDGE('',*,*,#3661,.F.);
#5029=ORIENTED_EDGE('',*,*,#3662,.T.);
#5030=ORIENTED_EDGE('',*,*,#3663,.F.);
#5031=ORIENTED_EDGE('',*,*,#3660,.F.);
#5032=ORIENTED_EDGE('',*,*,#3664,.F.);
#5033=ORIENTED_EDGE('',*,*,#3665,.T.);
#5034=ORIENTED_EDGE('',*,*,#3666,.T.);
#5035=ORIENTED_EDGE('',*,*,#3667,.T.);
#5036=ORIENTED_EDGE('',*,*,#3666,.F.);
#5037=ORIENTED_EDGE('',*,*,#3667,.F.);
#5038=ORIENTED_EDGE('',*,*,#3668,.T.);
#5039=ORIENTED_EDGE('',*,*,#3664,.T.);
#5040=ORIENTED_EDGE('',*,*,#3668,.F.);
#5041=ORIENTED_EDGE('',*,*,#3669,.T.);
#5042=ORIENTED_EDGE('',*,*,#3665,.F.);
#5043=ORIENTED_EDGE('',*,*,#3663,.T.);
#5044=ORIENTED_EDGE('',*,*,#3670,.T.);
#5045=ORIENTED_EDGE('',*,*,#3669,.F.);
#5046=ORIENTED_EDGE('',*,*,#3670,.F.);
#5047=ORIENTED_EDGE('',*,*,#3671,.F.);
#5048=ORIENTED_EDGE('',*,*,#3672,.T.);
#5049=ORIENTED_EDGE('',*,*,#3673,.T.);
#5050=ORIENTED_EDGE('',*,*,#3672,.F.);
#5051=ORIENTED_EDGE('',*,*,#3673,.F.);
#5052=ORIENTED_EDGE('',*,*,#3674,.F.);
#5053=ORIENTED_EDGE('',*,*,#3671,.T.);
#5054=ORIENTED_EDGE('',*,*,#3675,.F.);
#5055=ORIENTED_EDGE('',*,*,#3676,.F.);
#5056=ORIENTED_EDGE('',*,*,#3677,.T.);
#5057=ORIENTED_EDGE('',*,*,#3678,.T.);
#5058=ORIENTED_EDGE('',*,*,#3677,.F.);
#5059=ORIENTED_EDGE('',*,*,#3678,.F.);
#5060=ORIENTED_EDGE('',*,*,#3679,.T.);
#5061=ORIENTED_EDGE('',*,*,#3675,.T.);
#5062=ORIENTED_EDGE('',*,*,#3679,.F.);
#5063=ORIENTED_EDGE('',*,*,#3680,.T.);
#5064=ORIENTED_EDGE('',*,*,#3676,.T.);
#5065=ORIENTED_EDGE('',*,*,#3674,.T.);
#5066=ORIENTED_EDGE('',*,*,#3681,.T.);
#5067=ORIENTED_EDGE('',*,*,#3680,.F.);
#5068=ORIENTED_EDGE('',*,*,#3681,.F.);
#5069=ORIENTED_EDGE('',*,*,#3682,.F.);
#5070=ORIENTED_EDGE('',*,*,#3683,.F.);
#5071=ORIENTED_EDGE('',*,*,#3684,.F.);
#5072=ORIENTED_EDGE('',*,*,#3685,.T.);
#5073=ORIENTED_EDGE('',*,*,#3686,.F.);
#5074=ORIENTED_EDGE('',*,*,#3687,.T.);
#5075=ORIENTED_EDGE('',*,*,#3688,.F.);
#5076=ORIENTED_EDGE('',*,*,#3689,.F.);
#5077=ORIENTED_EDGE('',*,*,#3690,.T.);
#5078=ORIENTED_EDGE('',*,*,#3691,.T.);
#5079=ORIENTED_EDGE('',*,*,#3692,.F.);
#5080=ORIENTED_EDGE('',*,*,#3693,.T.);
#5081=ORIENTED_EDGE('',*,*,#3694,.F.);
#5082=ORIENTED_EDGE('',*,*,#3695,.F.);
#5083=ORIENTED_EDGE('',*,*,#3696,.F.);
#5084=ORIENTED_EDGE('',*,*,#3697,.F.);
#5085=ORIENTED_EDGE('',*,*,#3698,.F.);
#5086=ORIENTED_EDGE('',*,*,#3699,.F.);
#5087=ORIENTED_EDGE('',*,*,#3700,.F.);
#5088=ORIENTED_EDGE('',*,*,#3701,.F.);
#5089=ORIENTED_EDGE('',*,*,#3702,.F.);
#5090=ORIENTED_EDGE('',*,*,#3703,.F.);
#5091=ORIENTED_EDGE('',*,*,#3704,.F.);
#5092=ORIENTED_EDGE('',*,*,#3705,.F.);
#5093=ORIENTED_EDGE('',*,*,#3706,.F.);
#5094=ORIENTED_EDGE('',*,*,#3707,.F.);
#5095=ORIENTED_EDGE('',*,*,#3708,.F.);
#5096=ORIENTED_EDGE('',*,*,#3709,.F.);
#5097=ORIENTED_EDGE('',*,*,#3710,.F.);
#5098=ORIENTED_EDGE('',*,*,#3711,.F.);
#5099=ORIENTED_EDGE('',*,*,#3712,.F.);
#5100=ORIENTED_EDGE('',*,*,#3713,.F.);
#5101=ORIENTED_EDGE('',*,*,#3714,.T.);
#5102=ORIENTED_EDGE('',*,*,#3715,.T.);
#5103=ORIENTED_EDGE('',*,*,#3716,.F.);
#5104=ORIENTED_EDGE('',*,*,#3717,.T.);
#5105=ORIENTED_EDGE('',*,*,#3718,.F.);
#5106=ORIENTED_EDGE('',*,*,#3719,.F.);
#5107=ORIENTED_EDGE('',*,*,#3720,.F.);
#5108=ORIENTED_EDGE('',*,*,#3721,.F.);
#5109=ORIENTED_EDGE('',*,*,#3722,.F.);
#5110=ORIENTED_EDGE('',*,*,#3723,.F.);
#5111=ORIENTED_EDGE('',*,*,#3724,.F.);
#5112=ORIENTED_EDGE('',*,*,#3725,.F.);
#5113=ORIENTED_EDGE('',*,*,#3726,.F.);
#5114=ORIENTED_EDGE('',*,*,#3727,.F.);
#5115=ORIENTED_EDGE('',*,*,#3728,.F.);
#5116=ORIENTED_EDGE('',*,*,#3729,.F.);
#5117=ORIENTED_EDGE('',*,*,#3730,.F.);
#5118=ORIENTED_EDGE('',*,*,#3731,.F.);
#5119=ORIENTED_EDGE('',*,*,#3732,.F.);
#5120=ORIENTED_EDGE('',*,*,#3733,.F.);
#5121=ORIENTED_EDGE('',*,*,#3734,.F.);
#5122=ORIENTED_EDGE('',*,*,#3735,.F.);
#5123=ORIENTED_EDGE('',*,*,#3736,.F.);
#5124=ORIENTED_EDGE('',*,*,#3737,.F.);
#5125=ORIENTED_EDGE('',*,*,#3738,.F.);
#5126=ORIENTED_EDGE('',*,*,#3739,.F.);
#5127=ORIENTED_EDGE('',*,*,#3740,.F.);
#5128=ORIENTED_EDGE('',*,*,#3741,.F.);
#5129=ORIENTED_EDGE('',*,*,#3742,.F.);
#5130=ORIENTED_EDGE('',*,*,#3743,.F.);
#5131=ORIENTED_EDGE('',*,*,#3744,.F.);
#5132=ORIENTED_EDGE('',*,*,#3745,.F.);
#5133=ORIENTED_EDGE('',*,*,#3746,.F.);
#5134=ORIENTED_EDGE('',*,*,#3747,.F.);
#5135=ORIENTED_EDGE('',*,*,#3748,.F.);
#5136=ORIENTED_EDGE('',*,*,#3749,.F.);
#5137=ORIENTED_EDGE('',*,*,#3750,.F.);
#5138=ORIENTED_EDGE('',*,*,#3751,.F.);
#5139=ORIENTED_EDGE('',*,*,#3752,.F.);
#5140=ORIENTED_EDGE('',*,*,#3753,.F.);
#5141=ORIENTED_EDGE('',*,*,#3754,.F.);
#5142=ORIENTED_EDGE('',*,*,#3755,.F.);
#5143=ORIENTED_EDGE('',*,*,#3756,.F.);
#5144=ORIENTED_EDGE('',*,*,#3757,.F.);
#5145=ORIENTED_EDGE('',*,*,#3758,.F.);
#5146=ORIENTED_EDGE('',*,*,#3759,.T.);
#5147=ORIENTED_EDGE('',*,*,#3760,.T.);
#5148=ORIENTED_EDGE('',*,*,#3761,.T.);
#5149=ORIENTED_EDGE('',*,*,#3762,.F.);
#5150=ORIENTED_EDGE('',*,*,#3763,.T.);
#5151=ORIENTED_EDGE('',*,*,#3764,.F.);
#5152=ORIENTED_EDGE('',*,*,#3765,.F.);
#5153=ORIENTED_EDGE('',*,*,#3766,.T.);
#5154=ORIENTED_EDGE('',*,*,#3760,.F.);
#5155=ORIENTED_EDGE('',*,*,#3767,.F.);
#5156=ORIENTED_EDGE('',*,*,#3768,.F.);
#5157=ORIENTED_EDGE('',*,*,#3769,.T.);
#5158=ORIENTED_EDGE('',*,*,#3690,.F.);
#5159=ORIENTED_EDGE('',*,*,#3770,.F.);
#5160=ORIENTED_EDGE('',*,*,#3771,.F.);
#5161=ORIENTED_EDGE('',*,*,#3772,.T.);
#5162=ORIENTED_EDGE('',*,*,#3714,.F.);
#5163=ORIENTED_EDGE('',*,*,#3773,.F.);
#5164=ORIENTED_EDGE('',*,*,#3774,.F.);
#5165=ORIENTED_EDGE('',*,*,#3775,.T.);
#5166=ORIENTED_EDGE('',*,*,#3776,.F.);
#5167=ORIENTED_EDGE('',*,*,#3683,.T.);
#5168=ORIENTED_EDGE('',*,*,#3777,.F.);
#5169=ORIENTED_EDGE('',*,*,#3778,.F.);
#5170=ORIENTED_EDGE('',*,*,#3779,.F.);
#5171=ORIENTED_EDGE('',*,*,#3689,.T.);
#5172=ORIENTED_EDGE('',*,*,#3780,.F.);
#5173=ORIENTED_EDGE('',*,*,#3781,.F.);
#5174=ORIENTED_EDGE('',*,*,#3782,.F.);
#5175=ORIENTED_EDGE('',*,*,#3765,.T.);
#5176=ORIENTED_EDGE('',*,*,#3783,.F.);
#5177=ORIENTED_EDGE('',*,*,#3784,.F.);
#5178=ORIENTED_EDGE('',*,*,#3785,.F.);
#5179=ORIENTED_EDGE('',*,*,#3776,.T.);
#5180=ORIENTED_EDGE('',*,*,#3786,.T.);
#5181=ORIENTED_EDGE('',*,*,#3766,.F.);
#5182=ORIENTED_EDGE('',*,*,#3786,.F.);
#5183=ORIENTED_EDGE('',*,*,#3687,.F.);
#5184=ORIENTED_EDGE('',*,*,#3787,.T.);
#5185=ORIENTED_EDGE('',*,*,#3788,.T.);
#5186=ORIENTED_EDGE('',*,*,#3789,.T.);
#5187=ORIENTED_EDGE('',*,*,#3685,.F.);
#5188=ORIENTED_EDGE('',*,*,#3790,.T.);
#5189=ORIENTED_EDGE('',*,*,#3791,.T.);
#5190=ORIENTED_EDGE('',*,*,#3792,.T.);
#5191=ORIENTED_EDGE('',*,*,#3763,.F.);
#5192=ORIENTED_EDGE('',*,*,#3793,.T.);
#5193=ORIENTED_EDGE('',*,*,#3794,.T.);
#5194=ORIENTED_EDGE('',*,*,#3795,.T.);
#5195=ORIENTED_EDGE('',*,*,#3796,.F.);
#5196=ORIENTED_EDGE('',*,*,#3797,.F.);
#5197=ORIENTED_EDGE('',*,*,#3798,.F.);
#5198=ORIENTED_EDGE('',*,*,#3799,.F.);
#5199=ORIENTED_EDGE('',*,*,#3758,.T.);
#5200=ORIENTED_EDGE('',*,*,#3800,.F.);
#5201=ORIENTED_EDGE('',*,*,#3801,.F.);
#5202=ORIENTED_EDGE('',*,*,#3802,.F.);
#5203=ORIENTED_EDGE('',*,*,#3716,.T.);
#5204=ORIENTED_EDGE('',*,*,#3803,.F.);
#5205=ORIENTED_EDGE('',*,*,#3804,.F.);
#5206=ORIENTED_EDGE('',*,*,#3805,.F.);
#5207=ORIENTED_EDGE('',*,*,#3692,.T.);
#5208=ORIENTED_EDGE('',*,*,#3806,.F.);
#5209=ORIENTED_EDGE('',*,*,#3807,.F.);
#5210=ORIENTED_EDGE('',*,*,#3806,.T.);
#5211=ORIENTED_EDGE('',*,*,#3808,.T.);
#5212=ORIENTED_EDGE('',*,*,#3742,.T.);
#5213=ORIENTED_EDGE('',*,*,#3809,.F.);
#5214=ORIENTED_EDGE('',*,*,#3810,.T.);
#5215=ORIENTED_EDGE('',*,*,#3811,.T.);
#5216=ORIENTED_EDGE('',*,*,#3743,.T.);
#5217=ORIENTED_EDGE('',*,*,#3808,.F.);
#5218=ORIENTED_EDGE('',*,*,#3812,.F.);
#5219=ORIENTED_EDGE('',*,*,#3813,.F.);
#5220=ORIENTED_EDGE('',*,*,#3812,.T.);
#5221=ORIENTED_EDGE('',*,*,#3814,.T.);
#5222=ORIENTED_EDGE('',*,*,#3739,.T.);
#5223=ORIENTED_EDGE('',*,*,#3748,.T.);
#5224=ORIENTED_EDGE('',*,*,#3740,.T.);
#5225=ORIENTED_EDGE('',*,*,#3814,.F.);
#5226=ORIENTED_EDGE('',*,*,#3815,.F.);
#5227=ORIENTED_EDGE('',*,*,#3816,.F.);
#5228=ORIENTED_EDGE('',*,*,#3815,.T.);
#5229=ORIENTED_EDGE('',*,*,#3817,.T.);
#5230=ORIENTED_EDGE('',*,*,#3745,.T.);
#5231=ORIENTED_EDGE('',*,*,#3753,.T.);
#5232=ORIENTED_EDGE('',*,*,#3746,.T.);
#5233=ORIENTED_EDGE('',*,*,#3817,.F.);
#5234=ORIENTED_EDGE('',*,*,#3818,.F.);
#5235=ORIENTED_EDGE('',*,*,#3819,.F.);
#5236=ORIENTED_EDGE('',*,*,#3818,.T.);
#5237=ORIENTED_EDGE('',*,*,#3820,.T.);
#5238=ORIENTED_EDGE('',*,*,#3750,.T.);
#5239=ORIENTED_EDGE('',*,*,#3755,.T.);
#5240=ORIENTED_EDGE('',*,*,#3751,.T.);
#5241=ORIENTED_EDGE('',*,*,#3820,.F.);
#5242=ORIENTED_EDGE('',*,*,#3821,.T.);
#5243=ORIENTED_EDGE('',*,*,#3822,.F.);
#5244=ORIENTED_EDGE('',*,*,#3821,.F.);
#5245=ORIENTED_EDGE('',*,*,#3823,.T.);
#5246=ORIENTED_EDGE('',*,*,#3807,.T.);
#5247=ORIENTED_EDGE('',*,*,#3823,.F.);
#5248=ORIENTED_EDGE('',*,*,#3824,.T.);
#5249=ORIENTED_EDGE('',*,*,#3825,.F.);
#5250=ORIENTED_EDGE('',*,*,#3824,.F.);
#5251=ORIENTED_EDGE('',*,*,#3826,.T.);
#5252=ORIENTED_EDGE('',*,*,#3813,.T.);
#5253=ORIENTED_EDGE('',*,*,#3826,.F.);
#5254=ORIENTED_EDGE('',*,*,#3827,.T.);
#5255=ORIENTED_EDGE('',*,*,#3828,.F.);
#5256=ORIENTED_EDGE('',*,*,#3827,.F.);
#5257=ORIENTED_EDGE('',*,*,#3829,.T.);
#5258=ORIENTED_EDGE('',*,*,#3816,.T.);
#5259=ORIENTED_EDGE('',*,*,#3829,.F.);
#5260=ORIENTED_EDGE('',*,*,#3830,.F.);
#5261=ORIENTED_EDGE('',*,*,#3831,.T.);
#5262=ORIENTED_EDGE('',*,*,#3796,.T.);
#5263=ORIENTED_EDGE('',*,*,#3831,.F.);
#5264=ORIENTED_EDGE('',*,*,#3832,.T.);
#5265=ORIENTED_EDGE('',*,*,#3833,.T.);
#5266=ORIENTED_EDGE('',*,*,#3834,.T.);
#5267=ORIENTED_EDGE('',*,*,#3835,.T.);
#5268=ORIENTED_EDGE('',*,*,#3836,.T.);
#5269=ORIENTED_EDGE('',*,*,#3837,.T.);
#5270=ORIENTED_EDGE('',*,*,#3838,.T.);
#5271=ORIENTED_EDGE('',*,*,#3839,.T.);
#5272=ORIENTED_EDGE('',*,*,#3840,.T.);
#5273=ORIENTED_EDGE('',*,*,#3841,.T.);
#5274=ORIENTED_EDGE('',*,*,#3842,.T.);
#5275=ORIENTED_EDGE('',*,*,#3843,.T.);
#5276=ORIENTED_EDGE('',*,*,#3844,.T.);
#5277=ORIENTED_EDGE('',*,*,#3845,.T.);
#5278=ORIENTED_EDGE('',*,*,#3846,.T.);
#5279=ORIENTED_EDGE('',*,*,#3847,.T.);
#5280=ORIENTED_EDGE('',*,*,#3848,.T.);
#5281=ORIENTED_EDGE('',*,*,#3849,.T.);
#5282=ORIENTED_EDGE('',*,*,#3850,.T.);
#5283=ORIENTED_EDGE('',*,*,#3851,.T.);
#5284=ORIENTED_EDGE('',*,*,#3852,.T.);
#5285=ORIENTED_EDGE('',*,*,#3853,.T.);
#5286=ORIENTED_EDGE('',*,*,#3854,.T.);
#5287=ORIENTED_EDGE('',*,*,#3855,.T.);
#5288=ORIENTED_EDGE('',*,*,#3830,.T.);
#5289=ORIENTED_EDGE('',*,*,#3856,.T.);
#5290=ORIENTED_EDGE('',*,*,#3857,.F.);
#5291=ORIENTED_EDGE('',*,*,#3856,.F.);
#5292=ORIENTED_EDGE('',*,*,#3858,.T.);
#5293=ORIENTED_EDGE('',*,*,#3819,.T.);
#5294=ORIENTED_EDGE('',*,*,#3858,.F.);
#5295=ORIENTED_EDGE('',*,*,#3854,.F.);
#5296=ORIENTED_EDGE('',*,*,#3855,.F.);
#5297=ORIENTED_EDGE('',*,*,#3859,.T.);
#5298=ORIENTED_EDGE('',*,*,#3822,.T.);
#5299=ORIENTED_EDGE('',*,*,#3859,.F.);
#5300=ORIENTED_EDGE('',*,*,#3852,.F.);
#5301=ORIENTED_EDGE('',*,*,#3853,.F.);
#5302=ORIENTED_EDGE('',*,*,#3860,.T.);
#5303=ORIENTED_EDGE('',*,*,#3825,.T.);
#5304=ORIENTED_EDGE('',*,*,#3860,.F.);
#5305=ORIENTED_EDGE('',*,*,#3850,.F.);
#5306=ORIENTED_EDGE('',*,*,#3851,.F.);
#5307=ORIENTED_EDGE('',*,*,#3861,.T.);
#5308=ORIENTED_EDGE('',*,*,#3828,.T.);
#5309=ORIENTED_EDGE('',*,*,#3861,.F.);
#5310=ORIENTED_EDGE('',*,*,#3848,.F.);
#5311=ORIENTED_EDGE('',*,*,#3849,.F.);
#5312=ORIENTED_EDGE('',*,*,#3862,.T.);
#5313=ORIENTED_EDGE('',*,*,#3857,.T.);
#5314=ORIENTED_EDGE('',*,*,#3862,.F.);
#5315=ORIENTED_EDGE('',*,*,#3863,.F.);
#5316=ORIENTED_EDGE('',*,*,#3864,.F.);
#5317=ORIENTED_EDGE('',*,*,#3863,.T.);
#5318=ORIENTED_EDGE('',*,*,#3865,.T.);
#5319=ORIENTED_EDGE('',*,*,#3698,.T.);
#5320=ORIENTED_EDGE('',*,*,#3866,.F.);
#5321=ORIENTED_EDGE('',*,*,#3867,.T.);
#5322=ORIENTED_EDGE('',*,*,#3868,.T.);
#5323=ORIENTED_EDGE('',*,*,#3699,.T.);
#5324=ORIENTED_EDGE('',*,*,#3865,.F.);
#5325=ORIENTED_EDGE('',*,*,#3869,.F.);
#5326=ORIENTED_EDGE('',*,*,#3870,.F.);
#5327=ORIENTED_EDGE('',*,*,#3869,.T.);
#5328=ORIENTED_EDGE('',*,*,#3871,.T.);
#5329=ORIENTED_EDGE('',*,*,#3722,.T.);
#5330=ORIENTED_EDGE('',*,*,#3872,.F.);
#5331=ORIENTED_EDGE('',*,*,#3873,.T.);
#5332=ORIENTED_EDGE('',*,*,#3874,.T.);
#5333=ORIENTED_EDGE('',*,*,#3723,.T.);
#5334=ORIENTED_EDGE('',*,*,#3871,.F.);
#5335=ORIENTED_EDGE('',*,*,#3875,.F.);
#5336=ORIENTED_EDGE('',*,*,#3876,.F.);
#5337=ORIENTED_EDGE('',*,*,#3875,.T.);
#5338=ORIENTED_EDGE('',*,*,#3877,.T.);
#5339=ORIENTED_EDGE('',*,*,#3695,.T.);
#5340=ORIENTED_EDGE('',*,*,#3704,.T.);
#5341=ORIENTED_EDGE('',*,*,#3696,.T.);
#5342=ORIENTED_EDGE('',*,*,#3877,.F.);
#5343=ORIENTED_EDGE('',*,*,#3878,.F.);
#5344=ORIENTED_EDGE('',*,*,#3879,.F.);
#5345=ORIENTED_EDGE('',*,*,#3878,.T.);
#5346=ORIENTED_EDGE('',*,*,#3880,.T.);
#5347=ORIENTED_EDGE('',*,*,#3719,.T.);
#5348=ORIENTED_EDGE('',*,*,#3728,.T.);
#5349=ORIENTED_EDGE('',*,*,#3720,.T.);
#5350=ORIENTED_EDGE('',*,*,#3880,.F.);
#5351=ORIENTED_EDGE('',*,*,#3881,.F.);
#5352=ORIENTED_EDGE('',*,*,#3882,.F.);
#5353=ORIENTED_EDGE('',*,*,#3881,.T.);
#5354=ORIENTED_EDGE('',*,*,#3883,.T.);
#5355=ORIENTED_EDGE('',*,*,#3701,.T.);
#5356=ORIENTED_EDGE('',*,*,#3709,.T.);
#5357=ORIENTED_EDGE('',*,*,#3702,.T.);
#5358=ORIENTED_EDGE('',*,*,#3883,.F.);
#5359=ORIENTED_EDGE('',*,*,#3884,.F.);
#5360=ORIENTED_EDGE('',*,*,#3885,.F.);
#5361=ORIENTED_EDGE('',*,*,#3884,.T.);
#5362=ORIENTED_EDGE('',*,*,#3886,.T.);
#5363=ORIENTED_EDGE('',*,*,#3725,.T.);
#5364=ORIENTED_EDGE('',*,*,#3733,.T.);
#5365=ORIENTED_EDGE('',*,*,#3726,.T.);
#5366=ORIENTED_EDGE('',*,*,#3886,.F.);
#5367=ORIENTED_EDGE('',*,*,#3887,.F.);
#5368=ORIENTED_EDGE('',*,*,#3888,.F.);
#5369=ORIENTED_EDGE('',*,*,#3887,.T.);
#5370=ORIENTED_EDGE('',*,*,#3889,.T.);
#5371=ORIENTED_EDGE('',*,*,#3706,.T.);
#5372=ORIENTED_EDGE('',*,*,#3711,.T.);
#5373=ORIENTED_EDGE('',*,*,#3707,.T.);
#5374=ORIENTED_EDGE('',*,*,#3889,.F.);
#5375=ORIENTED_EDGE('',*,*,#3890,.F.);
#5376=ORIENTED_EDGE('',*,*,#3891,.F.);
#5377=ORIENTED_EDGE('',*,*,#3890,.T.);
#5378=ORIENTED_EDGE('',*,*,#3892,.T.);
#5379=ORIENTED_EDGE('',*,*,#3730,.T.);
#5380=ORIENTED_EDGE('',*,*,#3735,.T.);
#5381=ORIENTED_EDGE('',*,*,#3731,.T.);
#5382=ORIENTED_EDGE('',*,*,#3892,.F.);
#5383=ORIENTED_EDGE('',*,*,#3846,.F.);
#5384=ORIENTED_EDGE('',*,*,#3847,.F.);
#5385=ORIENTED_EDGE('',*,*,#3893,.T.);
#5386=ORIENTED_EDGE('',*,*,#3894,.F.);
#5387=ORIENTED_EDGE('',*,*,#3893,.F.);
#5388=ORIENTED_EDGE('',*,*,#3844,.F.);
#5389=ORIENTED_EDGE('',*,*,#3845,.F.);
#5390=ORIENTED_EDGE('',*,*,#3895,.T.);
#5391=ORIENTED_EDGE('',*,*,#3896,.F.);
#5392=ORIENTED_EDGE('',*,*,#3895,.F.);
#5393=ORIENTED_EDGE('',*,*,#3842,.F.);
#5394=ORIENTED_EDGE('',*,*,#3843,.F.);
#5395=ORIENTED_EDGE('',*,*,#3897,.T.);
#5396=ORIENTED_EDGE('',*,*,#3898,.F.);
#5397=ORIENTED_EDGE('',*,*,#3897,.F.);
#5398=ORIENTED_EDGE('',*,*,#3840,.F.);
#5399=ORIENTED_EDGE('',*,*,#3841,.F.);
#5400=ORIENTED_EDGE('',*,*,#3899,.T.);
#5401=ORIENTED_EDGE('',*,*,#3900,.F.);
#5402=ORIENTED_EDGE('',*,*,#3899,.F.);
#5403=ORIENTED_EDGE('',*,*,#3838,.F.);
#5404=ORIENTED_EDGE('',*,*,#3839,.F.);
#5405=ORIENTED_EDGE('',*,*,#3901,.T.);
#5406=ORIENTED_EDGE('',*,*,#3902,.F.);
#5407=ORIENTED_EDGE('',*,*,#3901,.F.);
#5408=ORIENTED_EDGE('',*,*,#3836,.F.);
#5409=ORIENTED_EDGE('',*,*,#3837,.F.);
#5410=ORIENTED_EDGE('',*,*,#3903,.T.);
#5411=ORIENTED_EDGE('',*,*,#3904,.F.);
#5412=ORIENTED_EDGE('',*,*,#3903,.F.);
#5413=ORIENTED_EDGE('',*,*,#3834,.F.);
#5414=ORIENTED_EDGE('',*,*,#3835,.F.);
#5415=ORIENTED_EDGE('',*,*,#3905,.T.);
#5416=ORIENTED_EDGE('',*,*,#3906,.F.);
#5417=ORIENTED_EDGE('',*,*,#3905,.F.);
#5418=ORIENTED_EDGE('',*,*,#3832,.F.);
#5419=ORIENTED_EDGE('',*,*,#3833,.F.);
#5420=ORIENTED_EDGE('',*,*,#3907,.T.);
#5421=ORIENTED_EDGE('',*,*,#3908,.F.);
#5422=ORIENTED_EDGE('',*,*,#3907,.F.);
#5423=ORIENTED_EDGE('',*,*,#3909,.T.);
#5424=ORIENTED_EDGE('',*,*,#3896,.T.);
#5425=ORIENTED_EDGE('',*,*,#3909,.F.);
#5426=ORIENTED_EDGE('',*,*,#3910,.T.);
#5427=ORIENTED_EDGE('',*,*,#3864,.T.);
#5428=ORIENTED_EDGE('',*,*,#3910,.F.);
#5429=ORIENTED_EDGE('',*,*,#3911,.T.);
#5430=ORIENTED_EDGE('',*,*,#3894,.T.);
#5431=ORIENTED_EDGE('',*,*,#3911,.F.);
#5432=ORIENTED_EDGE('',*,*,#3912,.T.);
#5433=ORIENTED_EDGE('',*,*,#3870,.T.);
#5434=ORIENTED_EDGE('',*,*,#3912,.F.);
#5435=ORIENTED_EDGE('',*,*,#3913,.T.);
#5436=ORIENTED_EDGE('',*,*,#3900,.T.);
#5437=ORIENTED_EDGE('',*,*,#3913,.F.);
#5438=ORIENTED_EDGE('',*,*,#3914,.T.);
#5439=ORIENTED_EDGE('',*,*,#3876,.T.);
#5440=ORIENTED_EDGE('',*,*,#3914,.F.);
#5441=ORIENTED_EDGE('',*,*,#3915,.T.);
#5442=ORIENTED_EDGE('',*,*,#3898,.T.);
#5443=ORIENTED_EDGE('',*,*,#3915,.F.);
#5444=ORIENTED_EDGE('',*,*,#3916,.T.);
#5445=ORIENTED_EDGE('',*,*,#3879,.T.);
#5446=ORIENTED_EDGE('',*,*,#3916,.F.);
#5447=ORIENTED_EDGE('',*,*,#3917,.T.);
#5448=ORIENTED_EDGE('',*,*,#3904,.T.);
#5449=ORIENTED_EDGE('',*,*,#3917,.F.);
#5450=ORIENTED_EDGE('',*,*,#3918,.T.);
#5451=ORIENTED_EDGE('',*,*,#3882,.T.);
#5452=ORIENTED_EDGE('',*,*,#3918,.F.);
#5453=ORIENTED_EDGE('',*,*,#3919,.T.);
#5454=ORIENTED_EDGE('',*,*,#3902,.T.);
#5455=ORIENTED_EDGE('',*,*,#3919,.F.);
#5456=ORIENTED_EDGE('',*,*,#3920,.T.);
#5457=ORIENTED_EDGE('',*,*,#3885,.T.);
#5458=ORIENTED_EDGE('',*,*,#3920,.F.);
#5459=ORIENTED_EDGE('',*,*,#3921,.T.);
#5460=ORIENTED_EDGE('',*,*,#3908,.T.);
#5461=ORIENTED_EDGE('',*,*,#3921,.F.);
#5462=ORIENTED_EDGE('',*,*,#3922,.T.);
#5463=ORIENTED_EDGE('',*,*,#3888,.T.);
#5464=ORIENTED_EDGE('',*,*,#3922,.F.);
#5465=ORIENTED_EDGE('',*,*,#3923,.T.);
#5466=ORIENTED_EDGE('',*,*,#3906,.T.);
#5467=ORIENTED_EDGE('',*,*,#3923,.F.);
#5468=ORIENTED_EDGE('',*,*,#3924,.T.);
#5469=ORIENTED_EDGE('',*,*,#3891,.T.);
#5470=ORIENTED_EDGE('',*,*,#3924,.F.);
#5471=ORIENTED_EDGE('',*,*,#3775,.F.);
#5472=ORIENTED_EDGE('',*,*,#3925,.F.);
#5473=ORIENTED_EDGE('',*,*,#3800,.T.);
#5474=ORIENTED_EDGE('',*,*,#3761,.F.);
#5475=ORIENTED_EDGE('',*,*,#3802,.T.);
#5476=ORIENTED_EDGE('',*,*,#3926,.F.);
#5477=ORIENTED_EDGE('',*,*,#3773,.T.);
#5478=ORIENTED_EDGE('',*,*,#3717,.F.);
#5479=ORIENTED_EDGE('',*,*,#3741,.T.);
#5480=ORIENTED_EDGE('',*,*,#3747,.T.);
#5481=ORIENTED_EDGE('',*,*,#3752,.T.);
#5482=ORIENTED_EDGE('',*,*,#3754,.T.);
#5483=ORIENTED_EDGE('',*,*,#3927,.F.);
#5484=ORIENTED_EDGE('',*,*,#3928,.T.);
#5485=ORIENTED_EDGE('',*,*,#3809,.T.);
#5486=ORIENTED_EDGE('',*,*,#3756,.T.);
#5487=ORIENTED_EDGE('',*,*,#3749,.T.);
#5488=ORIENTED_EDGE('',*,*,#3744,.T.);
#5489=ORIENTED_EDGE('',*,*,#3738,.T.);
#5490=ORIENTED_EDGE('',*,*,#3811,.F.);
#5491=ORIENTED_EDGE('',*,*,#3929,.T.);
#5492=ORIENTED_EDGE('',*,*,#3930,.T.);
#5493=ORIENTED_EDGE('',*,*,#3757,.T.);
#5494=ORIENTED_EDGE('',*,*,#3930,.F.);
#5495=ORIENTED_EDGE('',*,*,#3931,.T.);
#5496=ORIENTED_EDGE('',*,*,#3927,.T.);
#5497=ORIENTED_EDGE('',*,*,#3801,.T.);
#5498=ORIENTED_EDGE('',*,*,#3925,.T.);
#5499=ORIENTED_EDGE('',*,*,#3774,.T.);
#5500=ORIENTED_EDGE('',*,*,#3926,.T.);
#5501=ORIENTED_EDGE('',*,*,#3929,.F.);
#5502=ORIENTED_EDGE('',*,*,#3810,.F.);
#5503=ORIENTED_EDGE('',*,*,#3928,.F.);
#5504=ORIENTED_EDGE('',*,*,#3931,.F.);
#5505=ORIENTED_EDGE('',*,*,#3772,.F.);
#5506=ORIENTED_EDGE('',*,*,#3932,.F.);
#5507=ORIENTED_EDGE('',*,*,#3803,.T.);
#5508=ORIENTED_EDGE('',*,*,#3715,.F.);
#5509=ORIENTED_EDGE('',*,*,#3805,.T.);
#5510=ORIENTED_EDGE('',*,*,#3933,.F.);
#5511=ORIENTED_EDGE('',*,*,#3770,.T.);
#5512=ORIENTED_EDGE('',*,*,#3693,.F.);
#5513=ORIENTED_EDGE('',*,*,#3721,.T.);
#5514=ORIENTED_EDGE('',*,*,#3727,.T.);
#5515=ORIENTED_EDGE('',*,*,#3732,.T.);
#5516=ORIENTED_EDGE('',*,*,#3734,.T.);
#5517=ORIENTED_EDGE('',*,*,#3934,.F.);
#5518=ORIENTED_EDGE('',*,*,#3935,.T.);
#5519=ORIENTED_EDGE('',*,*,#3872,.T.);
#5520=ORIENTED_EDGE('',*,*,#3736,.T.);
#5521=ORIENTED_EDGE('',*,*,#3729,.T.);
#5522=ORIENTED_EDGE('',*,*,#3724,.T.);
#5523=ORIENTED_EDGE('',*,*,#3718,.T.);
#5524=ORIENTED_EDGE('',*,*,#3874,.F.);
#5525=ORIENTED_EDGE('',*,*,#3936,.T.);
#5526=ORIENTED_EDGE('',*,*,#3937,.T.);
#5527=ORIENTED_EDGE('',*,*,#3737,.T.);
#5528=ORIENTED_EDGE('',*,*,#3937,.F.);
#5529=ORIENTED_EDGE('',*,*,#3938,.T.);
#5530=ORIENTED_EDGE('',*,*,#3934,.T.);
#5531=ORIENTED_EDGE('',*,*,#3804,.T.);
#5532=ORIENTED_EDGE('',*,*,#3932,.T.);
#5533=ORIENTED_EDGE('',*,*,#3771,.T.);
#5534=ORIENTED_EDGE('',*,*,#3933,.T.);
#5535=ORIENTED_EDGE('',*,*,#3936,.F.);
#5536=ORIENTED_EDGE('',*,*,#3873,.F.);
#5537=ORIENTED_EDGE('',*,*,#3935,.F.);
#5538=ORIENTED_EDGE('',*,*,#3938,.F.);
#5539=ORIENTED_EDGE('',*,*,#3769,.F.);
#5540=ORIENTED_EDGE('',*,*,#3939,.F.);
#5541=ORIENTED_EDGE('',*,*,#3797,.T.);
#5542=ORIENTED_EDGE('',*,*,#3691,.F.);
#5543=ORIENTED_EDGE('',*,*,#3799,.T.);
#5544=ORIENTED_EDGE('',*,*,#3940,.F.);
#5545=ORIENTED_EDGE('',*,*,#3767,.T.);
#5546=ORIENTED_EDGE('',*,*,#3759,.F.);
#5547=ORIENTED_EDGE('',*,*,#3697,.T.);
#5548=ORIENTED_EDGE('',*,*,#3703,.T.);
#5549=ORIENTED_EDGE('',*,*,#3708,.T.);
#5550=ORIENTED_EDGE('',*,*,#3710,.T.);
#5551=ORIENTED_EDGE('',*,*,#3941,.F.);
#5552=ORIENTED_EDGE('',*,*,#3942,.T.);
#5553=ORIENTED_EDGE('',*,*,#3866,.T.);
#5554=ORIENTED_EDGE('',*,*,#3712,.T.);
#5555=ORIENTED_EDGE('',*,*,#3705,.T.);
#5556=ORIENTED_EDGE('',*,*,#3700,.T.);
#5557=ORIENTED_EDGE('',*,*,#3694,.T.);
#5558=ORIENTED_EDGE('',*,*,#3868,.F.);
#5559=ORIENTED_EDGE('',*,*,#3943,.T.);
#5560=ORIENTED_EDGE('',*,*,#3944,.T.);
#5561=ORIENTED_EDGE('',*,*,#3713,.T.);
#5562=ORIENTED_EDGE('',*,*,#3944,.F.);
#5563=ORIENTED_EDGE('',*,*,#3945,.T.);
#5564=ORIENTED_EDGE('',*,*,#3941,.T.);
#5565=ORIENTED_EDGE('',*,*,#3798,.T.);
#5566=ORIENTED_EDGE('',*,*,#3939,.T.);
#5567=ORIENTED_EDGE('',*,*,#3768,.T.);
#5568=ORIENTED_EDGE('',*,*,#3940,.T.);
#5569=ORIENTED_EDGE('',*,*,#3943,.F.);
#5570=ORIENTED_EDGE('',*,*,#3867,.F.);
#5571=ORIENTED_EDGE('',*,*,#3942,.F.);
#5572=ORIENTED_EDGE('',*,*,#3945,.F.);
#5573=ORIENTED_EDGE('',*,*,#3764,.T.);
#5574=ORIENTED_EDGE('',*,*,#3792,.F.);
#5575=ORIENTED_EDGE('',*,*,#3946,.T.);
#5576=ORIENTED_EDGE('',*,*,#3783,.T.);
#5577=ORIENTED_EDGE('',*,*,#3684,.T.);
#5578=ORIENTED_EDGE('',*,*,#3785,.T.);
#5579=ORIENTED_EDGE('',*,*,#3947,.F.);
#5580=ORIENTED_EDGE('',*,*,#3790,.F.);
#5581=ORIENTED_EDGE('',*,*,#3947,.T.);
#5582=ORIENTED_EDGE('',*,*,#3784,.T.);
#5583=ORIENTED_EDGE('',*,*,#3946,.F.);
#5584=ORIENTED_EDGE('',*,*,#3791,.F.);
#5585=ORIENTED_EDGE('',*,*,#3688,.T.);
#5586=ORIENTED_EDGE('',*,*,#3795,.F.);
#5587=ORIENTED_EDGE('',*,*,#3948,.T.);
#5588=ORIENTED_EDGE('',*,*,#3780,.T.);
#5589=ORIENTED_EDGE('',*,*,#3762,.T.);
#5590=ORIENTED_EDGE('',*,*,#3782,.T.);
#5591=ORIENTED_EDGE('',*,*,#3949,.F.);
#5592=ORIENTED_EDGE('',*,*,#3793,.F.);
#5593=ORIENTED_EDGE('',*,*,#3949,.T.);
#5594=ORIENTED_EDGE('',*,*,#3781,.T.);
#5595=ORIENTED_EDGE('',*,*,#3948,.F.);
#5596=ORIENTED_EDGE('',*,*,#3794,.F.);
#5597=ORIENTED_EDGE('',*,*,#3682,.T.);
#5598=ORIENTED_EDGE('',*,*,#3789,.F.);
#5599=ORIENTED_EDGE('',*,*,#3950,.T.);
#5600=ORIENTED_EDGE('',*,*,#3777,.T.);
#5601=ORIENTED_EDGE('',*,*,#3686,.T.);
#5602=ORIENTED_EDGE('',*,*,#3779,.T.);
#5603=ORIENTED_EDGE('',*,*,#3951,.F.);
#5604=ORIENTED_EDGE('',*,*,#3787,.F.);
#5605=ORIENTED_EDGE('',*,*,#3951,.T.);
#5606=ORIENTED_EDGE('',*,*,#3778,.T.);
#5607=ORIENTED_EDGE('',*,*,#3950,.F.);
#5608=ORIENTED_EDGE('',*,*,#3788,.F.);
#5609=ORIENTED_EDGE('',*,*,#3952,.F.);
#5610=ORIENTED_EDGE('',*,*,#3953,.T.);
#5611=ORIENTED_EDGE('',*,*,#3954,.T.);
#5612=ORIENTED_EDGE('',*,*,#3953,.F.);
#5613=ORIENTED_EDGE('',*,*,#3954,.F.);
#5614=ORIENTED_EDGE('',*,*,#3955,.T.);
#5615=ORIENTED_EDGE('',*,*,#3952,.T.);
#5616=ORIENTED_EDGE('',*,*,#3956,.F.);
#5617=ORIENTED_EDGE('',*,*,#3956,.T.);
#5618=ORIENTED_EDGE('',*,*,#3957,.T.);
#5619=ORIENTED_EDGE('',*,*,#3958,.F.);
#5620=ORIENTED_EDGE('',*,*,#3957,.F.);
#5621=ORIENTED_EDGE('',*,*,#3958,.T.);
#5622=ORIENTED_EDGE('',*,*,#3959,.F.);
#5623=ORIENTED_EDGE('',*,*,#3955,.F.);
#5624=ORIENTED_EDGE('',*,*,#3960,.T.);
#5625=ORIENTED_EDGE('',*,*,#3959,.T.);
#5626=ORIENTED_EDGE('',*,*,#3960,.F.);
#5627=PLANE('',#6260);
#5628=PLANE('',#6265);
#5629=PLANE('',#6288);
#5630=PLANE('',#6293);
#5631=PLANE('',#6295);
#5632=PLANE('',#6297);
#5633=PLANE('',#6298);
#5634=PLANE('',#6299);
#5635=PLANE('',#6300);
#5636=PLANE('',#6305);
#5637=PLANE('',#6306);
#5638=PLANE('',#6312);
#5639=PLANE('',#6315);
#5640=PLANE('',#6320);
#5641=PLANE('',#6324);
#5642=PLANE('',#6326);
#5643=PLANE('',#6329);
#5644=PLANE('',#6330);
#5645=PLANE('',#6331);
#5646=PLANE('',#6352);
#5647=PLANE('',#6354);
#5648=PLANE('',#6360);
#5649=PLANE('',#6362);
#5650=PLANE('',#6371);
#5651=PLANE('',#6373);
#5652=PLANE('',#6378);
#5653=PLANE('',#6380);
#5654=PLANE('',#6385);
#5655=PLANE('',#6387);
#5656=PLANE('',#6407);
#5657=PLANE('',#6422);
#5658=PLANE('',#6425);
#5659=PLANE('',#6431);
#5660=PLANE('',#6433);
#5661=PLANE('',#6442);
#5662=PLANE('',#6444);
#5663=PLANE('',#6449);
#5664=PLANE('',#6451);
#5665=PLANE('',#6456);
#5666=PLANE('',#6458);
#5667=PLANE('',#6479);
#5668=PLANE('',#6482);
#5669=PLANE('',#6485);
#5670=PLANE('',#6488);
#5671=PLANE('',#6489);
#5672=PLANE('',#6492);
#5673=PLANE('',#6495);
#5674=PLANE('',#6498);
#5675=PLANE('',#6499);
#5676=PLANE('',#6502);
#5677=PLANE('',#6505);
#5678=PLANE('',#6508);
#5679=PLANE('',#6518);
#5680=PLANE('',#6529);
#5681=PLANE('',#6540);
#5682=PLANE('',#6545);
#5683=PLANE('',#6547);
#5684=PLANE('',#6551);
#5685=PLANE('',#6554);
#5686=PLANE('',#6565);
#5687=PLANE('',#6570);
#5688=PLANE('',#6579);
#5689=PLANE('',#6582);
#5690=PLANE('',#6583);
#5691=PLANE('',#6584);
#5692=PLANE('',#6585);
#5693=PLANE('',#6586);
#5694=PLANE('',#6587);
#5695=PLANE('',#6588);
#5696=PLANE('',#6589);
#5697=PLANE('',#6590);
#5698=PLANE('',#6591);
#5699=PLANE('',#6592);
#5700=PLANE('',#6593);
#5701=PLANE('',#6594);
#5702=PLANE('',#6595);
#5703=PLANE('',#6596);
#5704=PLANE('',#6597);
#5705=PLANE('',#6598);
#5706=PLANE('',#6599);
#5707=PLANE('',#6600);
#5708=PLANE('',#6601);
#5709=PLANE('',#6602);
#5710=PLANE('',#6603);
#5711=PLANE('',#6604);
#5712=PLANE('',#6605);
#5713=PLANE('',#6606);
#5714=PLANE('',#6607);
#5715=PLANE('',#6608);
#5716=PLANE('',#6613);
#5717=PLANE('',#6615);
#5718=PLANE('',#6621);
#5719=PLANE('',#6628);
#5720=PLANE('',#6630);
#5721=PLANE('',#6636);
#5722=PLANE('',#6643);
#5723=PLANE('',#6645);
#5724=PLANE('',#6651);
#5725=PLANE('',#6658);
#5726=PLANE('',#6660);
#5727=PLANE('',#6666);
#5728=PLANE('',#6700);
#5729=PLANE('',#6705);
#5730=PLANE('',#6708);
#5731=PLANE('',#6710);
#5732=PLANE('',#6714);
#5733=PLANE('',#6718);
#5734=PLANE('',#6722);
#5735=PLANE('',#6726);
#5736=PLANE('',#6730);
#5737=PLANE('',#6734);
#5738=PLANE('',#6738);
#5739=PLANE('',#6744);
#5740=PLANE('',#6745);
#5741=PLANE('',#6753);
#5742=PLANE('',#6757);
#5743=PLANE('',#6761);
#5744=PLANE('',#6765);
#5745=PLANE('',#6769);
#5746=PLANE('',#6773);
#5747=PLANE('',#6777);
#5748=PLANE('',#6781);
#5749=PLANE('',#6801);
#5750=PLANE('',#6804);
#5751=PLANE('',#6807);
#5752=PLANE('',#6810);
#5753=PLANE('',#6813);
#5754=PLANE('',#6816);
#5755=PLANE('',#6819);
#5756=PLANE('',#6822);
#5757=PLANE('',#6825);
#5758=PLANE('',#6826);
#5759=PLANE('',#6827);
#5760=PLANE('',#6828);
#5761=PLANE('',#6830);
#5762=PLANE('',#6831);
#5763=PLANE('',#6832);
#5764=PLANE('',#6833);
#5765=PLANE('',#6835);
#5766=PLANE('',#6836);
#5767=PLANE('',#6837);
#5768=PLANE('',#6838);
#5769=PLANE('',#6840);
#5770=PLANE('',#6841);
#5771=PLANE('',#6842);
#5772=PLANE('',#6843);
#5773=PLANE('',#6844);
#5774=PLANE('',#6845);
#5775=PLANE('',#6846);
#5776=PLANE('',#6847);
#5777=PLANE('',#6848);
#5778=PLANE('',#6893);
#5779=PLANE('',#6895);
#5780=PLANE('',#6899);
#5781=ADVANCED_FACE('',(#732,#627,#628,#629),#5627,.T.);
#5782=ADVANCED_FACE('',(#733,#630,#631,#632,#633,#634,#635,#636,#637),#5628,
 .T.);
#5783=ADVANCED_FACE('',(#734,#638,#639),#477,.F.);
#5784=ADVANCED_FACE('',(#735),#478,.F.);
#5785=ADVANCED_FACE('',(#736),#479,.T.);
#5786=ADVANCED_FACE('',(#737,#640,#641,#642),#5629,.T.);
#5787=ADVANCED_FACE('',(#738),#5630,.T.);
#5788=ADVANCED_FACE('',(#739),#5631,.T.);
#5789=ADVANCED_FACE('',(#740),#5632,.T.);
#5790=ADVANCED_FACE('',(#741),#5633,.T.);
#5791=ADVANCED_FACE('',(#742),#5634,.T.);
#5792=ADVANCED_FACE('',(#743),#5635,.T.);
#5793=ADVANCED_FACE('',(#744),#480,.F.);
#5794=ADVANCED_FACE('',(#745),#481,.F.);
#5795=ADVANCED_FACE('',(#746),#482,.T.);
#5796=ADVANCED_FACE('',(#747),#279,.T.);
#5797=ADVANCED_FACE('',(#748),#280,.T.);
#5798=ADVANCED_FACE('',(#749),#281,.T.);
#5799=ADVANCED_FACE('',(#750),#282,.F.);
#5800=ADVANCED_FACE('',(#751),#483,.T.);
#5801=ADVANCED_FACE('',(#752),#283,.F.);
#5802=ADVANCED_FACE('',(#753),#5636,.T.);
#5803=ADVANCED_FACE('',(#754),#5637,.T.);
#5804=ADVANCED_FACE('',(#755),#484,.T.);
#5805=ADVANCED_FACE('',(#756),#485,.T.);
#5806=ADVANCED_FACE('',(#757),#486,.F.);
#5807=ADVANCED_FACE('',(#758),#487,.F.);
#5808=ADVANCED_FACE('',(#759),#488,.T.);
#5809=ADVANCED_FACE('',(#760),#284,.F.);
#5810=ADVANCED_FACE('',(#761),#285,.F.);
#5811=ADVANCED_FACE('',(#762),#286,.F.);
#5812=ADVANCED_FACE('',(#763),#287,.T.);
#5813=ADVANCED_FACE('',(#764),#288,.T.);
#5814=ADVANCED_FACE('',(#765),#5638,.F.);
#5815=ADVANCED_FACE('',(#766),#5639,.F.);
#5816=ADVANCED_FACE('',(#767),#489,.T.);
#5817=ADVANCED_FACE('',(#768,#643),#5640,.T.);
#5818=ADVANCED_FACE('',(#769),#490,.T.);
#5819=ADVANCED_FACE('',(#770,#644),#5641,.T.);
#5820=ADVANCED_FACE('',(#771),#491,.F.);
#5821=ADVANCED_FACE('',(#772,#645),#5642,.T.);
#5822=ADVANCED_FACE('',(#773),#492,.T.);
#5823=ADVANCED_FACE('',(#774),#5643,.F.);
#5824=ADVANCED_FACE('',(#775),#5644,.F.);
#5825=ADVANCED_FACE('',(#776),#5645,.T.);
#5826=ADVANCED_FACE('',(#777),#493,.F.);
#5827=ADVANCED_FACE('',(#778),#494,.F.);
#5828=ADVANCED_FACE('',(#779),#495,.F.);
#5829=ADVANCED_FACE('',(#780),#496,.F.);
#5830=ADVANCED_FACE('',(#781),#497,.F.);
#5831=ADVANCED_FACE('',(#782),#498,.F.);
#5832=ADVANCED_FACE('',(#783,#646,#647,#648,#649,#650,#651,#652),#499,.T.);
#5833=ADVANCED_FACE('',(#784),#5646,.T.);
#5834=ADVANCED_FACE('',(#785,#653),#5647,.F.);
#5835=ADVANCED_FACE('',(#786),#219,.T.);
#5836=ADVANCED_FACE('',(#787),#220,.T.);
#5837=ADVANCED_FACE('',(#788),#221,.T.);
#5838=ADVANCED_FACE('',(#789),#222,.T.);
#5839=ADVANCED_FACE('',(#790),#500,.T.);
#5840=ADVANCED_FACE('',(#791),#5648,.T.);
#5841=ADVANCED_FACE('',(#792),#5649,.F.);
#5842=ADVANCED_FACE('',(#793),#501,.F.);
#5843=ADVANCED_FACE('',(#794),#199,.F.);
#5844=ADVANCED_FACE('',(#795),#200,.F.);
#5845=ADVANCED_FACE('',(#796),#502,.F.);
#5846=ADVANCED_FACE('',(#797),#503,.T.);
#5847=ADVANCED_FACE('',(#798),#5650,.T.);
#5848=ADVANCED_FACE('',(#799),#5651,.F.);
#5849=ADVANCED_FACE('',(#800),#504,.T.);
#5850=ADVANCED_FACE('',(#801),#5652,.T.);
#5851=ADVANCED_FACE('',(#802),#5653,.F.);
#5852=ADVANCED_FACE('',(#803),#505,.T.);
#5853=ADVANCED_FACE('',(#804),#5654,.T.);
#5854=ADVANCED_FACE('',(#805),#5655,.F.);
#5855=ADVANCED_FACE('',(#806),#506,.F.);
#5856=ADVANCED_FACE('',(#807),#201,.F.);
#5857=ADVANCED_FACE('',(#808),#202,.F.);
#5858=ADVANCED_FACE('',(#809),#507,.F.);
#5859=ADVANCED_FACE('',(#810),#508,.F.);
#5860=ADVANCED_FACE('',(#811),#203,.F.);
#5861=ADVANCED_FACE('',(#812),#204,.F.);
#5862=ADVANCED_FACE('',(#813),#509,.F.);
#5863=ADVANCED_FACE('',(#814),#510,.F.);
#5864=ADVANCED_FACE('',(#815),#205,.F.);
#5865=ADVANCED_FACE('',(#816),#206,.F.);
#5866=ADVANCED_FACE('',(#817),#511,.F.);
#5867=ADVANCED_FACE('',(#818),#207,.T.);
#5868=ADVANCED_FACE('',(#819),#208,.T.);
#5869=ADVANCED_FACE('',(#820),#512,.F.);
#5870=ADVANCED_FACE('',(#821),#5656,.T.);
#5871=ADVANCED_FACE('',(#822,#654,#655,#656,#657,#658,#659,#660),#513,.T.);
#5872=ADVANCED_FACE('',(#823,#661),#5657,.T.);
#5873=ADVANCED_FACE('',(#824,#662),#5658,.F.);
#5874=ADVANCED_FACE('',(#825),#223,.T.);
#5875=ADVANCED_FACE('',(#826),#224,.T.);
#5876=ADVANCED_FACE('',(#827),#225,.T.);
#5877=ADVANCED_FACE('',(#828),#226,.T.);
#5878=ADVANCED_FACE('',(#829),#514,.T.);
#5879=ADVANCED_FACE('',(#830),#5659,.T.);
#5880=ADVANCED_FACE('',(#831),#5660,.F.);
#5881=ADVANCED_FACE('',(#832),#515,.F.);
#5882=ADVANCED_FACE('',(#833),#209,.F.);
#5883=ADVANCED_FACE('',(#834),#210,.F.);
#5884=ADVANCED_FACE('',(#835),#516,.F.);
#5885=ADVANCED_FACE('',(#836),#517,.T.);
#5886=ADVANCED_FACE('',(#837),#5661,.T.);
#5887=ADVANCED_FACE('',(#838),#5662,.F.);
#5888=ADVANCED_FACE('',(#839),#518,.T.);
#5889=ADVANCED_FACE('',(#840),#5663,.T.);
#5890=ADVANCED_FACE('',(#841),#5664,.F.);
#5891=ADVANCED_FACE('',(#842),#519,.T.);
#5892=ADVANCED_FACE('',(#843),#5665,.T.);
#5893=ADVANCED_FACE('',(#844),#5666,.F.);
#5894=ADVANCED_FACE('',(#845),#520,.F.);
#5895=ADVANCED_FACE('',(#846),#211,.F.);
#5896=ADVANCED_FACE('',(#847),#212,.F.);
#5897=ADVANCED_FACE('',(#848),#521,.F.);
#5898=ADVANCED_FACE('',(#849),#522,.F.);
#5899=ADVANCED_FACE('',(#850),#213,.F.);
#5900=ADVANCED_FACE('',(#851),#214,.F.);
#5901=ADVANCED_FACE('',(#852),#523,.F.);
#5902=ADVANCED_FACE('',(#853),#524,.F.);
#5903=ADVANCED_FACE('',(#854),#215,.F.);
#5904=ADVANCED_FACE('',(#855),#216,.F.);
#5905=ADVANCED_FACE('',(#856),#525,.F.);
#5906=ADVANCED_FACE('',(#857),#217,.T.);
#5907=ADVANCED_FACE('',(#858),#218,.T.);
#5908=ADVANCED_FACE('',(#859),#526,.F.);
#5909=ADVANCED_FACE('',(#860),#5667,.T.);
#5910=ADVANCED_FACE('',(#861),#5668,.T.);
#5911=ADVANCED_FACE('',(#862),#527,.F.);
#5912=ADVANCED_FACE('',(#863),#5669,.T.);
#5913=ADVANCED_FACE('',(#864),#528,.T.);
#5914=ADVANCED_FACE('',(#865),#5670,.F.);
#5915=ADVANCED_FACE('',(#866),#5671,.T.);
#5916=ADVANCED_FACE('',(#867),#5672,.T.);
#5917=ADVANCED_FACE('',(#868),#529,.F.);
#5918=ADVANCED_FACE('',(#869),#5673,.T.);
#5919=ADVANCED_FACE('',(#870),#530,.T.);
#5920=ADVANCED_FACE('',(#871),#5674,.F.);
#5921=ADVANCED_FACE('',(#872),#5675,.T.);
#5922=ADVANCED_FACE('',(#873),#5676,.T.);
#5923=ADVANCED_FACE('',(#874),#531,.F.);
#5924=ADVANCED_FACE('',(#875),#5677,.T.);
#5925=ADVANCED_FACE('',(#876),#532,.T.);
#5926=ADVANCED_FACE('',(#877),#5678,.F.);
#5927=ADVANCED_FACE('',(#878),#533,.T.);
#5928=ADVANCED_FACE('',(#879),#534,.T.);
#5929=ADVANCED_FACE('',(#880),#535,.T.);
#5930=ADVANCED_FACE('',(#881,#663),#5679,.T.);
#5931=ADVANCED_FACE('',(#882),#536,.T.);
#5932=ADVANCED_FACE('',(#883),#537,.T.);
#5933=ADVANCED_FACE('',(#884),#538,.T.);
#5934=ADVANCED_FACE('',(#885,#664),#5680,.T.);
#5935=ADVANCED_FACE('',(#886),#539,.T.);
#5936=ADVANCED_FACE('',(#887),#540,.T.);
#5937=ADVANCED_FACE('',(#888),#541,.T.);
#5938=ADVANCED_FACE('',(#889,#665),#5681,.T.);
#5939=ADVANCED_FACE('',(#890,#666,#667),#542,.T.);
#5940=ADVANCED_FACE('',(#891,#668),#5682,.T.);
#5941=ADVANCED_FACE('',(#892,#669),#5683,.F.);
#5942=ADVANCED_FACE('',(#893),#543,.F.);
#5943=ADVANCED_FACE('',(#894),#5684,.T.);
#5944=ADVANCED_FACE('',(#895),#544,.T.);
#5945=ADVANCED_FACE('',(#896,#670),#5685,.T.);
#5946=ADVANCED_FACE('',(#897),#545,.T.);
#5947=ADVANCED_FACE('',(#898),#546,.F.);
#5948=ADVANCED_FACE('',(#899),#191,.T.);
#5949=ADVANCED_FACE('',(#900),#547,.T.);
#5950=ADVANCED_FACE('',(#901),#548,.T.);
#5951=ADVANCED_FACE('',(#902,#671),#5686,.T.);
#5952=ADVANCED_FACE('',(#903),#549,.T.);
#5953=ADVANCED_FACE('',(#904,#672),#5687,.T.);
#5954=ADVANCED_FACE('',(#905),#550,.T.);
#5955=ADVANCED_FACE('',(#906),#551,.F.);
#5956=ADVANCED_FACE('',(#907),#552,.F.);
#5957=ADVANCED_FACE('',(#908),#192,.T.);
#5958=ADVANCED_FACE('',(#909),#193,.T.);
#5959=ADVANCED_FACE('',(#910),#5688,.F.);
#5960=ADVANCED_FACE('',(#911,#673,#674),#553,.F.);
#5961=ADVANCED_FACE('',(#912),#5689,.T.);
#5962=ADVANCED_FACE('',(#913),#5690,.T.);
#5963=ADVANCED_FACE('',(#914),#5691,.F.);
#5964=ADVANCED_FACE('',(#915),#5692,.T.);
#5965=ADVANCED_FACE('',(#916),#5693,.T.);
#5966=ADVANCED_FACE('',(#917),#5694,.F.);
#5967=ADVANCED_FACE('',(#918),#5695,.T.);
#5968=ADVANCED_FACE('',(#919),#5696,.T.);
#5969=ADVANCED_FACE('',(#920),#5697,.F.);
#5970=ADVANCED_FACE('',(#921),#5698,.T.);
#5971=ADVANCED_FACE('',(#922),#5699,.T.);
#5972=ADVANCED_FACE('',(#923),#5700,.F.);
#5973=ADVANCED_FACE('',(#924),#5701,.T.);
#5974=ADVANCED_FACE('',(#925),#5702,.T.);
#5975=ADVANCED_FACE('',(#926),#5703,.F.);
#5976=ADVANCED_FACE('',(#927),#5704,.T.);
#5977=ADVANCED_FACE('',(#928),#5705,.T.);
#5978=ADVANCED_FACE('',(#929),#5706,.F.);
#5979=ADVANCED_FACE('',(#930),#5707,.T.);
#5980=ADVANCED_FACE('',(#931),#5708,.T.);
#5981=ADVANCED_FACE('',(#932),#5709,.F.);
#5982=ADVANCED_FACE('',(#933),#5710,.T.);
#5983=ADVANCED_FACE('',(#934),#5711,.T.);
#5984=ADVANCED_FACE('',(#935),#5712,.F.);
#5985=ADVANCED_FACE('',(#936),#5713,.T.);
#5986=ADVANCED_FACE('',(#937),#5714,.T.);
#5987=ADVANCED_FACE('',(#938),#5715,.F.);
#5988=ADVANCED_FACE('',(#939),#554,.T.);
#5989=ADVANCED_FACE('',(#940,#675),#5716,.T.);
#5990=ADVANCED_FACE('',(#941,#676),#5717,.F.);
#5991=ADVANCED_FACE('',(#942),#555,.F.);
#5992=ADVANCED_FACE('',(#943),#194,.F.);
#5993=ADVANCED_FACE('',(#944,#677),#5718,.T.);
#5994=ADVANCED_FACE('',(#945),#556,.T.);
#5995=ADVANCED_FACE('',(#946),#557,.T.);
#5996=ADVANCED_FACE('',(#947,#678),#5719,.T.);
#5997=ADVANCED_FACE('',(#948,#679),#5720,.F.);
#5998=ADVANCED_FACE('',(#949),#558,.F.);
#5999=ADVANCED_FACE('',(#950),#195,.F.);
#6000=ADVANCED_FACE('',(#951,#680),#5721,.T.);
#6001=ADVANCED_FACE('',(#952),#559,.T.);
#6002=ADVANCED_FACE('',(#953),#560,.T.);
#6003=ADVANCED_FACE('',(#954,#681),#5722,.T.);
#6004=ADVANCED_FACE('',(#955,#682),#5723,.F.);
#6005=ADVANCED_FACE('',(#956),#561,.F.);
#6006=ADVANCED_FACE('',(#957),#196,.F.);
#6007=ADVANCED_FACE('',(#958,#683),#5724,.T.);
#6008=ADVANCED_FACE('',(#959),#562,.T.);
#6009=ADVANCED_FACE('',(#960),#563,.T.);
#6010=ADVANCED_FACE('',(#961,#684),#5725,.F.);
#6011=ADVANCED_FACE('',(#962,#685),#5726,.T.);
#6012=ADVANCED_FACE('',(#963),#564,.F.);
#6013=ADVANCED_FACE('',(#964),#197,.F.);
#6014=ADVANCED_FACE('',(#965,#686),#5727,.T.);
#6015=ADVANCED_FACE('',(#966),#565,.T.);
#6016=ADVANCED_FACE('',(#967),#566,.F.);
#6017=ADVANCED_FACE('',(#968),#567,.F.);
#6018=ADVANCED_FACE('',(#969),#568,.T.);
#6019=ADVANCED_FACE('',(#970),#569,.T.);
#6020=ADVANCED_FACE('',(#971),#570,.T.);
#6021=ADVANCED_FACE('',(#972),#571,.T.);
#6022=ADVANCED_FACE('',(#973),#572,.T.);
#6023=ADVANCED_FACE('',(#974),#573,.T.);
#6024=ADVANCED_FACE('',(#975),#574,.T.);
#6025=ADVANCED_FACE('',(#976),#575,.T.);
#6026=ADVANCED_FACE('',(#977),#576,.T.);
#6027=ADVANCED_FACE('',(#978),#577,.T.);
#6028=ADVANCED_FACE('',(#979),#578,.T.);
#6029=ADVANCED_FACE('',(#980),#579,.T.);
#6030=ADVANCED_FACE('',(#981),#580,.T.);
#6031=ADVANCED_FACE('',(#982),#581,.T.);
#6032=ADVANCED_FACE('',(#983),#582,.T.);
#6033=ADVANCED_FACE('',(#984),#583,.F.);
#6034=ADVANCED_FACE('',(#985,#687),#5728,.T.);
#6035=ADVANCED_FACE('',(#986,#688),#5729,.F.);
#6036=ADVANCED_FACE('',(#987),#584,.T.);
#6037=ADVANCED_FACE('',(#988,#689),#5730,.F.);
#6038=ADVANCED_FACE('',(#989),#5731,.T.);
#6039=ADVANCED_FACE('',(#990,#690),#5732,.F.);
#6040=ADVANCED_FACE('',(#991),#585,.T.);
#6041=ADVANCED_FACE('',(#992,#691),#5733,.F.);
#6042=ADVANCED_FACE('',(#993),#586,.T.);
#6043=ADVANCED_FACE('',(#994,#692),#5734,.F.);
#6044=ADVANCED_FACE('',(#995),#587,.T.);
#6045=ADVANCED_FACE('',(#996,#693),#5735,.F.);
#6046=ADVANCED_FACE('',(#997),#588,.T.);
#6047=ADVANCED_FACE('',(#998,#694),#5736,.T.);
#6048=ADVANCED_FACE('',(#999),#589,.F.);
#6049=ADVANCED_FACE('',(#1000,#695),#5737,.T.);
#6050=ADVANCED_FACE('',(#1001),#590,.F.);
#6051=ADVANCED_FACE('',(#1002,#696),#5738,.T.);
#6052=ADVANCED_FACE('',(#1003),#591,.F.);
#6053=ADVANCED_FACE('',(#1004,#697,#698,#699,#700,#701,#702,#703,#704,#705,
#706,#707,#708),#592,.F.);
#6054=ADVANCED_FACE('',(#1005),#5739,.F.);
#6055=ADVANCED_FACE('',(#1006,#709),#5740,.T.);
#6056=ADVANCED_FACE('',(#1007),#593,.F.);
#6057=ADVANCED_FACE('',(#1008),#594,.F.);
#6058=ADVANCED_FACE('',(#1009),#595,.F.);
#6059=ADVANCED_FACE('',(#1010),#596,.F.);
#6060=ADVANCED_FACE('',(#1011),#597,.F.);
#6061=ADVANCED_FACE('',(#1012,#710),#5741,.F.);
#6062=ADVANCED_FACE('',(#1013),#598,.T.);
#6063=ADVANCED_FACE('',(#1014,#711),#5742,.F.);
#6064=ADVANCED_FACE('',(#1015),#599,.T.);
#6065=ADVANCED_FACE('',(#1016,#712),#5743,.F.);
#6066=ADVANCED_FACE('',(#1017),#600,.T.);
#6067=ADVANCED_FACE('',(#1018,#713),#5744,.F.);
#6068=ADVANCED_FACE('',(#1019),#601,.T.);
#6069=ADVANCED_FACE('',(#1020,#714),#5745,.F.);
#6070=ADVANCED_FACE('',(#1021),#602,.T.);
#6071=ADVANCED_FACE('',(#1022,#715),#5746,.F.);
#6072=ADVANCED_FACE('',(#1023),#603,.T.);
#6073=ADVANCED_FACE('',(#1024,#716),#5747,.F.);
#6074=ADVANCED_FACE('',(#1025),#604,.T.);
#6075=ADVANCED_FACE('',(#1026,#717),#5748,.F.);
#6076=ADVANCED_FACE('',(#1027),#605,.T.);
#6077=ADVANCED_FACE('',(#1028),#606,.F.);
#6078=ADVANCED_FACE('',(#1029),#607,.F.);
#6079=ADVANCED_FACE('',(#1030),#608,.F.);
#6080=ADVANCED_FACE('',(#1031),#609,.F.);
#6081=ADVANCED_FACE('',(#1032),#610,.F.);
#6082=ADVANCED_FACE('',(#1033),#611,.F.);
#6083=ADVANCED_FACE('',(#1034),#612,.F.);
#6084=ADVANCED_FACE('',(#1035),#613,.F.);
#6085=ADVANCED_FACE('',(#1036,#718),#5749,.T.);
#6086=ADVANCED_FACE('',(#1037),#614,.F.);
#6087=ADVANCED_FACE('',(#1038,#719),#5750,.T.);
#6088=ADVANCED_FACE('',(#1039),#615,.F.);
#6089=ADVANCED_FACE('',(#1040,#720),#5751,.T.);
#6090=ADVANCED_FACE('',(#1041),#616,.F.);
#6091=ADVANCED_FACE('',(#1042,#721),#5752,.T.);
#6092=ADVANCED_FACE('',(#1043),#617,.F.);
#6093=ADVANCED_FACE('',(#1044,#722),#5753,.T.);
#6094=ADVANCED_FACE('',(#1045),#618,.F.);
#6095=ADVANCED_FACE('',(#1046,#723),#5754,.T.);
#6096=ADVANCED_FACE('',(#1047),#619,.F.);
#6097=ADVANCED_FACE('',(#1048,#724),#5755,.T.);
#6098=ADVANCED_FACE('',(#1049),#620,.F.);
#6099=ADVANCED_FACE('',(#1050,#725),#5756,.T.);
#6100=ADVANCED_FACE('',(#1051),#621,.F.);
#6101=ADVANCED_FACE('',(#1052),#5757,.F.);
#6102=ADVANCED_FACE('',(#1053),#5758,.F.);
#6103=ADVANCED_FACE('',(#1054),#5759,.T.);
#6104=ADVANCED_FACE('',(#1055),#5760,.T.);
#6105=ADVANCED_FACE('',(#1056),#289,.T.);
#6106=ADVANCED_FACE('',(#1057,#726),#622,.T.);
#6107=ADVANCED_FACE('',(#1058),#5761,.F.);
#6108=ADVANCED_FACE('',(#1059),#5762,.F.);
#6109=ADVANCED_FACE('',(#1060),#5763,.T.);
#6110=ADVANCED_FACE('',(#1061),#5764,.T.);
#6111=ADVANCED_FACE('',(#1062),#290,.T.);
#6112=ADVANCED_FACE('',(#1063,#727),#623,.T.);
#6113=ADVANCED_FACE('',(#1064),#5765,.F.);
#6114=ADVANCED_FACE('',(#1065),#5766,.F.);
#6115=ADVANCED_FACE('',(#1066),#5767,.T.);
#6116=ADVANCED_FACE('',(#1067),#5768,.T.);
#6117=ADVANCED_FACE('',(#1068),#291,.T.);
#6118=ADVANCED_FACE('',(#1069,#728),#624,.T.);
#6119=ADVANCED_FACE('',(#1070),#5769,.F.);
#6120=ADVANCED_FACE('',(#1071),#5770,.F.);
#6121=ADVANCED_FACE('',(#1072),#5771,.F.);
#6122=ADVANCED_FACE('',(#1073),#5772,.F.);
#6123=ADVANCED_FACE('',(#1074),#5773,.F.);
#6124=ADVANCED_FACE('',(#1075),#5774,.F.);
#6125=ADVANCED_FACE('',(#1076),#5775,.F.);
#6126=ADVANCED_FACE('',(#1077),#5776,.F.);
#6127=ADVANCED_FACE('',(#1078),#5777,.F.);
#6128=ADVANCED_FACE('',(#1079),#198,.T.);
#6129=ADVANCED_FACE('',(#1080,#729),#5778,.F.);
#6130=ADVANCED_FACE('',(#1081,#730),#5779,.T.);
#6131=ADVANCED_FACE('',(#1082),#625,.T.);
#6132=ADVANCED_FACE('',(#1083,#731),#5780,.T.);
#6133=ADVANCED_FACE('',(#1084),#626,.F.);
#6134=CLOSED_SHELL('',(#5781,#5782,#5783,#5784,#5785,#5786,#5787,#5788,
#5789,#5790,#5791,#5792,#5793,#5794,#5795,#5796,#5797,#5798,#5799,#5800,
#5801,#5802,#5803,#5804,#5805,#5806,#5807,#5808,#5809,#5810,#5811,#5812,
#5813,#5814,#5815,#5816,#5817,#5818,#5819,#5820,#5821,#5822,#5823,#5824,
#5825,#5826,#5827,#5828,#5829,#5830,#5831));
#6135=CLOSED_SHELL('',(#5832,#5833,#5834,#5835,#5836,#5837,#5838,#5839,
#5840,#5841,#5842,#5843,#5844,#5845,#5846,#5847,#5848,#5849,#5850,#5851,
#5852,#5853,#5854,#5855,#5856,#5857,#5858,#5859,#5860,#5861,#5862,#5863,
#5864,#5865,#5866,#5867,#5868,#5869,#5870));
#6136=CLOSED_SHELL('',(#5871,#5872,#5873,#5874,#5875,#5876,#5877,#5878,
#5879,#5880,#5881,#5882,#5883,#5884,#5885,#5886,#5887,#5888,#5889,#5890,
#5891,#5892,#5893,#5894,#5895,#5896,#5897,#5898,#5899,#5900,#5901,#5902,
#5903,#5904,#5905,#5906,#5907,#5908));
#6137=CLOSED_SHELL('',(#5909,#5910,#5911,#5912,#5913,#5914));
#6138=CLOSED_SHELL('',(#5915,#5916,#5917,#5918,#5919,#5920));
#6139=CLOSED_SHELL('',(#5921,#5922,#5923,#5924,#5925,#5926));
#6140=CLOSED_SHELL('',(#5927,#5928,#5929,#5930,#5931,#5932,#5933,#5934,
#5935,#5936,#5937,#5938,#5939,#5940,#5941,#5942,#5943,#5944,#5945,#5946,
#5947,#5948,#5949,#5950,#5951,#5952,#5953,#5954,#5955,#5956,#5957,#5958,
#5959,#5960,#5961,#5962,#5963,#5964,#5965,#5966,#5967,#5968,#5969,#5970,
#5971,#5972,#5973,#5974,#5975,#5976,#5977,#5978,#5979,#5980,#5981,#5982,
#5983,#5984,#5985,#5986,#5987));
#6141=CLOSED_SHELL('',(#5988,#5989,#5990,#5991,#5992,#5993,#5994));
#6142=CLOSED_SHELL('',(#5995,#5996,#5997,#5998,#5999,#6000,#6001));
#6143=CLOSED_SHELL('',(#6002,#6003,#6004,#6005,#6006,#6007,#6008));
#6144=CLOSED_SHELL('',(#6009,#6010,#6011,#6012,#6013,#6014,#6015));
#6145=CLOSED_SHELL('',(#6016,#6017,#6018,#6019,#6020,#6021,#6022,#6023,
#6024,#6025,#6026,#6027,#6028,#6029,#6030,#6031,#6032,#6033,#6034,#6035,
#6036,#6037,#6038,#6039,#6040,#6041,#6042,#6043,#6044,#6045,#6046,#6047,
#6048,#6049,#6050,#6051,#6052,#6053,#6054,#6055,#6056,#6057,#6058,#6059,
#6060,#6061,#6062,#6063,#6064,#6065,#6066,#6067,#6068,#6069,#6070,#6071,
#6072,#6073,#6074,#6075,#6076,#6077,#6078,#6079,#6080,#6081,#6082,#6083,
#6084,#6085,#6086,#6087,#6088,#6089,#6090,#6091,#6092,#6093,#6094,#6095,
#6096,#6097,#6098,#6099,#6100,#6101,#6102,#6103,#6104,#6105,#6106,#6107,
#6108,#6109,#6110,#6111,#6112,#6113,#6114,#6115,#6116,#6117,#6118,#6119,
#6120,#6121,#6122,#6123,#6124,#6125,#6126,#6127));
#6146=CLOSED_SHELL('',(#6128,#6129,#6130,#6131,#6132,#6133));
#6147=DERIVED_UNIT_ELEMENT(#6167,1.);
#6148=DERIVED_UNIT_ELEMENT(#14127,-3.);
#6149=DERIVED_UNIT_ELEMENT(#6167,1.);
#6150=DERIVED_UNIT_ELEMENT(#14127,-3.);
#6151=DERIVED_UNIT_ELEMENT(#6167,1.);
#6152=DERIVED_UNIT_ELEMENT(#14127,-3.);
#6153=DERIVED_UNIT_ELEMENT(#6167,1.);
#6154=DERIVED_UNIT_ELEMENT(#14127,-3.);
#6155=DERIVED_UNIT_ELEMENT(#6167,1.);
#6156=DERIVED_UNIT_ELEMENT(#14127,-3.);
#6157=DERIVED_UNIT_ELEMENT(#6167,1.);
#6158=DERIVED_UNIT_ELEMENT(#14127,-3.);
#6159=DERIVED_UNIT_ELEMENT(#6167,1.);
#6160=DERIVED_UNIT_ELEMENT(#14127,-3.);
#6161=DERIVED_UNIT_ELEMENT(#6167,1.);
#6162=DERIVED_UNIT_ELEMENT(#14127,-3.);
#6163=DERIVED_UNIT_ELEMENT(#6167,1.);
#6164=DERIVED_UNIT_ELEMENT(#14127,-3.);
#6165=DERIVED_UNIT_ELEMENT(#6167,1.);
#6166=DERIVED_UNIT_ELEMENT(#14127,-3.);
#6167=(
MASS_UNIT()
NAMED_UNIT(*)
SI_UNIT(.KILO.,.GRAM.)
);
#6168=DERIVED_UNIT((#6147,#6148));
#6169=DERIVED_UNIT((#6149,#6150));
#6170=DERIVED_UNIT((#6151,#6152));
#6171=DERIVED_UNIT((#6153,#6154));
#6172=DERIVED_UNIT((#6155,#6156));
#6173=DERIVED_UNIT((#6157,#6158));
#6174=DERIVED_UNIT((#6159,#6160));
#6175=DERIVED_UNIT((#6161,#6162));
#6176=DERIVED_UNIT((#6163,#6164));
#6177=DERIVED_UNIT((#6165,#6166));
#6178=MEASURE_REPRESENTATION_ITEM('density measure',
POSITIVE_RATIO_MEASURE(7850.),#6168);
#6179=MEASURE_REPRESENTATION_ITEM('density measure',
POSITIVE_RATIO_MEASURE(7850.),#6169);
#6180=MEASURE_REPRESENTATION_ITEM('density measure',
POSITIVE_RATIO_MEASURE(7850.),#6170);
#6181=MEASURE_REPRESENTATION_ITEM('density measure',
POSITIVE_RATIO_MEASURE(7850.),#6171);
#6182=MEASURE_REPRESENTATION_ITEM('density measure',
POSITIVE_RATIO_MEASURE(7850.),#6172);
#6183=MEASURE_REPRESENTATION_ITEM('density measure',
POSITIVE_RATIO_MEASURE(7850.),#6173);
#6184=MEASURE_REPRESENTATION_ITEM('density measure',
POSITIVE_RATIO_MEASURE(7850.),#6174);
#6185=MEASURE_REPRESENTATION_ITEM('density measure',
POSITIVE_RATIO_MEASURE(7850.),#6175);
#6186=MEASURE_REPRESENTATION_ITEM('density measure',
POSITIVE_RATIO_MEASURE(7850.),#6176);
#6187=MEASURE_REPRESENTATION_ITEM('density measure',
POSITIVE_RATIO_MEASURE(7850.),#6177);
#6188=PROPERTY_DEFINITION_REPRESENTATION(#6238,#6208);
#6189=PROPERTY_DEFINITION_REPRESENTATION(#6239,#6209);
#6190=PROPERTY_DEFINITION_REPRESENTATION(#6240,#6210);
#6191=PROPERTY_DEFINITION_REPRESENTATION(#6241,#6211);
#6192=PROPERTY_DEFINITION_REPRESENTATION(#6242,#6212);
#6193=PROPERTY_DEFINITION_REPRESENTATION(#6243,#6213);
#6194=PROPERTY_DEFINITION_REPRESENTATION(#6244,#6214);
#6195=PROPERTY_DEFINITION_REPRESENTATION(#6245,#6215);
#6196=PROPERTY_DEFINITION_REPRESENTATION(#6246,#6216);
#6197=PROPERTY_DEFINITION_REPRESENTATION(#6247,#6217);
#6198=PROPERTY_DEFINITION_REPRESENTATION(#6248,#6218);
#6199=PROPERTY_DEFINITION_REPRESENTATION(#6249,#6219);
#6200=PROPERTY_DEFINITION_REPRESENTATION(#6250,#6220);
#6201=PROPERTY_DEFINITION_REPRESENTATION(#6251,#6221);
#6202=PROPERTY_DEFINITION_REPRESENTATION(#6252,#6222);
#6203=PROPERTY_DEFINITION_REPRESENTATION(#6253,#6223);
#6204=PROPERTY_DEFINITION_REPRESENTATION(#6254,#6224);
#6205=PROPERTY_DEFINITION_REPRESENTATION(#6255,#6225);
#6206=PROPERTY_DEFINITION_REPRESENTATION(#6256,#6226);
#6207=PROPERTY_DEFINITION_REPRESENTATION(#6257,#6227);
#6208=REPRESENTATION('material name',(#6228),#14114);
#6209=REPRESENTATION('density',(#6178),#14114);
#6210=REPRESENTATION('material name',(#6229),#14115);
#6211=REPRESENTATION('density',(#6179),#14115);
#6212=REPRESENTATION('material name',(#6230),#14116);
#6213=REPRESENTATION('density',(#6180),#14116);
#6214=REPRESENTATION('material name',(#6231),#14118);
#6215=REPRESENTATION('density',(#6181),#14118);
#6216=REPRESENTATION('material name',(#6232),#14119);
#6217=REPRESENTATION('density',(#6182),#14119);
#6218=REPRESENTATION('material name',(#6233),#14120);
#6219=REPRESENTATION('density',(#6183),#14120);
#6220=REPRESENTATION('material name',(#6234),#14121);
#6221=REPRESENTATION('density',(#6184),#14121);
#6222=REPRESENTATION('material name',(#6235),#14122);
#6223=REPRESENTATION('density',(#6185),#14122);
#6224=REPRESENTATION('material name',(#6236),#14123);
#6225=REPRESENTATION('density',(#6186),#14123);
#6226=REPRESENTATION('material name',(#6237),#14124);
#6227=REPRESENTATION('density',(#6187),#14124);
#6228=DESCRIPTIVE_REPRESENTATION_ITEM('Steel','Steel');
#6229=DESCRIPTIVE_REPRESENTATION_ITEM('Steel','Steel');
#6230=DESCRIPTIVE_REPRESENTATION_ITEM('Steel','Steel');
#6231=DESCRIPTIVE_REPRESENTATION_ITEM('Steel','Steel');
#6232=DESCRIPTIVE_REPRESENTATION_ITEM('Steel','Steel');
#6233=DESCRIPTIVE_REPRESENTATION_ITEM('Steel','Steel');
#6234=DESCRIPTIVE_REPRESENTATION_ITEM('Steel','Steel');
#6235=DESCRIPTIVE_REPRESENTATION_ITEM('Steel','Steel');
#6236=DESCRIPTIVE_REPRESENTATION_ITEM('Steel','Steel');
#6237=DESCRIPTIVE_REPRESENTATION_ITEM('Steel','Steel');
#6238=PROPERTY_DEFINITION('material property','material name',#14213);
#6239=PROPERTY_DEFINITION('material property','density of part',#14213);
#6240=PROPERTY_DEFINITION('material property','material name',#14214);
#6241=PROPERTY_DEFINITION('material property','density of part',#14214);
#6242=PROPERTY_DEFINITION('material property','material name',#14215);
#6243=PROPERTY_DEFINITION('material property','density of part',#14215);
#6244=PROPERTY_DEFINITION('material property','material name',#14217);
#6245=PROPERTY_DEFINITION('material property','density of part',#14217);
#6246=PROPERTY_DEFINITION('material property','material name',#14218);
#6247=PROPERTY_DEFINITION('material property','density of part',#14218);
#6248=PROPERTY_DEFINITION('material property','material name',#14219);
#6249=PROPERTY_DEFINITION('material property','density of part',#14219);
#6250=PROPERTY_DEFINITION('material property','material name',#14220);
#6251=PROPERTY_DEFINITION('material property','density of part',#14220);
#6252=PROPERTY_DEFINITION('material property','material name',#14221);
#6253=PROPERTY_DEFINITION('material property','density of part',#14221);
#6254=PROPERTY_DEFINITION('material property','material name',#14222);
#6255=PROPERTY_DEFINITION('material property','density of part',#14222);
#6256=PROPERTY_DEFINITION('material property','material name',#14223);
#6257=PROPERTY_DEFINITION('material property','density of part',#14223);
#6258=AXIS2_PLACEMENT_3D('',#8593,#6907,#6908);
#6259=AXIS2_PLACEMENT_3D('',#8594,#6909,#6910);
#6260=AXIS2_PLACEMENT_3D('',#8595,#6911,#6912);
#6261=AXIS2_PLACEMENT_3D('',#8608,#6918,#6919);
#6262=AXIS2_PLACEMENT_3D('',#8613,#6922,#6923);
#6263=AXIS2_PLACEMENT_3D('',#8615,#6924,#6925);
#6264=AXIS2_PLACEMENT_3D('',#8617,#6926,#6927);
#6265=AXIS2_PLACEMENT_3D('',#8618,#6928,#6929);
#6266=AXIS2_PLACEMENT_3D('',#8621,#6930,#6931);
#6267=AXIS2_PLACEMENT_3D('',#8623,#6932,#6933);
#6268=AXIS2_PLACEMENT_3D('',#8625,#6934,#6935);
#6269=AXIS2_PLACEMENT_3D('',#8627,#6936,#6937);
#6270=AXIS2_PLACEMENT_3D('',#8629,#6938,#6939);
#6271=AXIS2_PLACEMENT_3D('',#8631,#6940,#6941);
#6272=AXIS2_PLACEMENT_3D('',#8633,#6942,#6943);
#6273=AXIS2_PLACEMENT_3D('',#8634,#6944,#6945);
#6274=AXIS2_PLACEMENT_3D('',#8644,#6950,#6951);
#6275=AXIS2_PLACEMENT_3D('',#8646,#6952,#6953);
#6276=AXIS2_PLACEMENT_3D('',#8648,#6954,#6955);
#6277=AXIS2_PLACEMENT_3D('',#8650,#6956,#6957);
#6278=AXIS2_PLACEMENT_3D('',#8652,#6958,#6959);
#6279=AXIS2_PLACEMENT_3D('',#8654,#6960,#6961);
#6280=AXIS2_PLACEMENT_3D('',#8663,#6966,#6967);
#6281=AXIS2_PLACEMENT_3D('',#8665,#6968,#6969);
#6282=AXIS2_PLACEMENT_3D('',#8668,#6971,#6972);
#6283=AXIS2_PLACEMENT_3D('',#8825,#6973,#6974);
#6284=AXIS2_PLACEMENT_3D('',#8827,#6975,#6976);
#6285=AXIS2_PLACEMENT_3D('',#8829,#6978,#6979);
#6286=AXIS2_PLACEMENT_3D('',#8874,#6982,#6983);
#6287=AXIS2_PLACEMENT_3D('',#8905,#6986,#6987);
#6288=AXIS2_PLACEMENT_3D('',#8906,#6988,#6989);
#6289=AXIS2_PLACEMENT_3D('',#8917,#6994,#6995);
#6290=AXIS2_PLACEMENT_3D('',#8924,#6999,#7000);
#6291=AXIS2_PLACEMENT_3D('',#8926,#7001,#7002);
#6292=AXIS2_PLACEMENT_3D('',#8928,#7003,#7004);
#6293=AXIS2_PLACEMENT_3D('',#8929,#7005,#7006);
#6294=AXIS2_PLACEMENT_3D('',#8932,#7007,#7008);
#6295=AXIS2_PLACEMENT_3D('',#9119,#7011,#7012);
#6296=AXIS2_PLACEMENT_3D('',#9124,#7015,#7016);
#6297=AXIS2_PLACEMENT_3D('',#9306,#7017,#7018);
#6298=AXIS2_PLACEMENT_3D('',#9313,#7021,#7022);
#6299=AXIS2_PLACEMENT_3D('',#9320,#7025,#7026);
#6300=AXIS2_PLACEMENT_3D('',#9327,#7028,#7029);
#6301=AXIS2_PLACEMENT_3D('',#9336,#7031,#7032);
#6302=AXIS2_PLACEMENT_3D('',#9387,#7035,#7036);
#6303=AXIS2_PLACEMENT_3D('',#9438,#7039,#7040);
#6304=AXIS2_PLACEMENT_3D('',#9732,#7044,#7045);
#6305=AXIS2_PLACEMENT_3D('',#9778,#7049,#7050);
#6306=AXIS2_PLACEMENT_3D('',#9780,#7052,#7053);
#6307=AXIS2_PLACEMENT_3D('',#9782,#7055,#7056);
#6308=AXIS2_PLACEMENT_3D('',#9784,#7058,#7059);
#6309=AXIS2_PLACEMENT_3D('',#9786,#7061,#7062);
#6310=AXIS2_PLACEMENT_3D('',#9835,#7064,#7065);
#6311=AXIS2_PLACEMENT_3D('',#9884,#7067,#7068);
#6312=AXIS2_PLACEMENT_3D('',#10148,#7071,#7072);
#6313=AXIS2_PLACEMENT_3D('',#10150,#7073,#7074);
#6314=AXIS2_PLACEMENT_3D('',#10151,#7075,#7076);
#6315=AXIS2_PLACEMENT_3D('',#10152,#7077,#7078);
#6316=AXIS2_PLACEMENT_3D('',#10154,#7079,#7080);
#6317=AXIS2_PLACEMENT_3D('',#10155,#7081,#7082);
#6318=AXIS2_PLACEMENT_3D('',#10156,#7083,#7084);
#6319=AXIS2_PLACEMENT_3D('',#10159,#7086,#7087);
#6320=AXIS2_PLACEMENT_3D('',#10160,#7088,#7089);
#6321=AXIS2_PLACEMENT_3D('',#10162,#7090,#7091);
#6322=AXIS2_PLACEMENT_3D('',#10163,#7092,#7093);
#6323=AXIS2_PLACEMENT_3D('',#10166,#7095,#7096);
#6324=AXIS2_PLACEMENT_3D('',#10167,#7097,#7098);
#6325=AXIS2_PLACEMENT_3D('',#10168,#7099,#7100);
#6326=AXIS2_PLACEMENT_3D('',#10170,#7102,#7103);
#6327=AXIS2_PLACEMENT_3D('',#10172,#7104,#7105);
#6328=AXIS2_PLACEMENT_3D('',#10173,#7106,#7107);
#6329=AXIS2_PLACEMENT_3D('',#10175,#7109,#7110);
#6330=AXIS2_PLACEMENT_3D('',#10176,#7111,#7112);
#6331=AXIS2_PLACEMENT_3D('',#10177,#7113,#7114);
#6332=AXIS2_PLACEMENT_3D('',#10178,#7115,#7116);
#6333=AXIS2_PLACEMENT_3D('',#10180,#7118,#7119);
#6334=AXIS2_PLACEMENT_3D('',#10182,#7121,#7122);
#6335=AXIS2_PLACEMENT_3D('',#10184,#7124,#7125);
#6336=AXIS2_PLACEMENT_3D('',#10186,#7127,#7128);
#6337=AXIS2_PLACEMENT_3D('',#10188,#7130,#7131);
#6338=AXIS2_PLACEMENT_3D('',#10190,#7133,#7134);
#6339=AXIS2_PLACEMENT_3D('',#10191,#7135,#7136);
#6340=AXIS2_PLACEMENT_3D('',#10194,#7137,#7138);
#6341=AXIS2_PLACEMENT_3D('',#10195,#7139,#7140);
#6342=AXIS2_PLACEMENT_3D('',#10233,#7143,#7144);
#6343=AXIS2_PLACEMENT_3D('',#10234,#7145,#7146);
#6344=AXIS2_PLACEMENT_3D('',#10264,#7148,#7149);
#6345=AXIS2_PLACEMENT_3D('',#10267,#7151,#7152);
#6346=AXIS2_PLACEMENT_3D('',#10272,#7154,#7155);
#6347=AXIS2_PLACEMENT_3D('',#10275,#7157,#7158);
#6348=AXIS2_PLACEMENT_3D('',#10280,#7160,#7161);
#6349=AXIS2_PLACEMENT_3D('',#10283,#7163,#7164);
#6350=AXIS2_PLACEMENT_3D('',#10288,#7166,#7167);
#6351=AXIS2_PLACEMENT_3D('',#10291,#7169,#7170);
#6352=AXIS2_PLACEMENT_3D('',#10427,#7171,#7172);
#6353=AXIS2_PLACEMENT_3D('',#10429,#7173,#7174);
#6354=AXIS2_PLACEMENT_3D('',#10430,#7175,#7176);
#6355=AXIS2_PLACEMENT_3D('',#10432,#7177,#7178);
#6356=AXIS2_PLACEMENT_3D('',#10434,#7179,#7180);
#6357=AXIS2_PLACEMENT_3D('',#10495,#7181,#7182);
#6358=AXIS2_PLACEMENT_3D('',#10498,#7183,#7184);
#6359=AXIS2_PLACEMENT_3D('',#10516,#7186,#7187);
#6360=AXIS2_PLACEMENT_3D('',#10532,#7189,#7190);
#6361=AXIS2_PLACEMENT_3D('',#10533,#7191,#7192);
#6362=AXIS2_PLACEMENT_3D('',#10534,#7193,#7194);
#6363=AXIS2_PLACEMENT_3D('',#10535,#7195,#7196);
#6364=AXIS2_PLACEMENT_3D('',#10536,#7197,#7198);
#6365=AXIS2_PLACEMENT_3D('',#10557,#7199,#7200);
#6366=AXIS2_PLACEMENT_3D('',#10568,#7201,#7202);
#6367=AXIS2_PLACEMENT_3D('',#10579,#7203,#7204);
#6368=AXIS2_PLACEMENT_3D('',#10580,#7205,#7206);
#6369=AXIS2_PLACEMENT_3D('',#10583,#7207,#7208);
#6370=AXIS2_PLACEMENT_3D('',#10601,#7210,#7211);
#6371=AXIS2_PLACEMENT_3D('',#10617,#7213,#7214);
#6372=AXIS2_PLACEMENT_3D('',#10618,#7215,#7216);
#6373=AXIS2_PLACEMENT_3D('',#10619,#7217,#7218);
#6374=AXIS2_PLACEMENT_3D('',#10620,#7219,#7220);
#6375=AXIS2_PLACEMENT_3D('',#10621,#7221,#7222);
#6376=AXIS2_PLACEMENT_3D('',#10624,#7223,#7224);
#6377=AXIS2_PLACEMENT_3D('',#10642,#7226,#7227);
#6378=AXIS2_PLACEMENT_3D('',#10658,#7229,#7230);
#6379=AXIS2_PLACEMENT_3D('',#10659,#7231,#7232);
#6380=AXIS2_PLACEMENT_3D('',#10660,#7233,#7234);
#6381=AXIS2_PLACEMENT_3D('',#10661,#7235,#7236);
#6382=AXIS2_PLACEMENT_3D('',#10662,#7237,#7238);
#6383=AXIS2_PLACEMENT_3D('',#10665,#7239,#7240);
#6384=AXIS2_PLACEMENT_3D('',#10683,#7242,#7243);
#6385=AXIS2_PLACEMENT_3D('',#10699,#7245,#7246);
#6386=AXIS2_PLACEMENT_3D('',#10700,#7247,#7248);
#6387=AXIS2_PLACEMENT_3D('',#10701,#7249,#7250);
#6388=AXIS2_PLACEMENT_3D('',#10702,#7251,#7252);
#6389=AXIS2_PLACEMENT_3D('',#10703,#7253,#7254);
#6390=AXIS2_PLACEMENT_3D('',#10724,#7255,#7256);
#6391=AXIS2_PLACEMENT_3D('',#10735,#7257,#7258);
#6392=AXIS2_PLACEMENT_3D('',#10746,#7259,#7260);
#6393=AXIS2_PLACEMENT_3D('',#10747,#7261,#7262);
#6394=AXIS2_PLACEMENT_3D('',#10768,#7263,#7264);
#6395=AXIS2_PLACEMENT_3D('',#10779,#7265,#7266);
#6396=AXIS2_PLACEMENT_3D('',#10790,#7267,#7268);
#6397=AXIS2_PLACEMENT_3D('',#10791,#7269,#7270);
#6398=AXIS2_PLACEMENT_3D('',#10812,#7271,#7272);
#6399=AXIS2_PLACEMENT_3D('',#10823,#7273,#7274);
#6400=AXIS2_PLACEMENT_3D('',#10834,#7275,#7276);
#6401=AXIS2_PLACEMENT_3D('',#10835,#7277,#7278);
#6402=AXIS2_PLACEMENT_3D('',#10836,#7279,#7280);
#6403=AXIS2_PLACEMENT_3D('',#10837,#7281,#7282);
#6404=AXIS2_PLACEMENT_3D('',#10838,#7283,#7284);
#6405=AXIS2_PLACEMENT_3D('',#10839,#7285,#7286);
#6406=AXIS2_PLACEMENT_3D('',#10842,#7288,#7289);
#6407=AXIS2_PLACEMENT_3D('',#10843,#7290,#7291);
#6408=AXIS2_PLACEMENT_3D('',#10844,#7292,#7293);
#6409=AXIS2_PLACEMENT_3D('',#10845,#7294,#7295);
#6410=AXIS2_PLACEMENT_3D('',#10848,#7296,#7297);
#6411=AXIS2_PLACEMENT_3D('',#10849,#7298,#7299);
#6412=AXIS2_PLACEMENT_3D('',#10887,#7302,#7303);
#6413=AXIS2_PLACEMENT_3D('',#10888,#7304,#7305);
#6414=AXIS2_PLACEMENT_3D('',#10918,#7307,#7308);
#6415=AXIS2_PLACEMENT_3D('',#10921,#7310,#7311);
#6416=AXIS2_PLACEMENT_3D('',#10926,#7313,#7314);
#6417=AXIS2_PLACEMENT_3D('',#10929,#7316,#7317);
#6418=AXIS2_PLACEMENT_3D('',#10934,#7319,#7320);
#6419=AXIS2_PLACEMENT_3D('',#10937,#7322,#7323);
#6420=AXIS2_PLACEMENT_3D('',#10942,#7325,#7326);
#6421=AXIS2_PLACEMENT_3D('',#10945,#7328,#7329);
#6422=AXIS2_PLACEMENT_3D('',#11081,#7330,#7331);
#6423=AXIS2_PLACEMENT_3D('',#11083,#7332,#7333);
#6424=AXIS2_PLACEMENT_3D('',#11085,#7334,#7335);
#6425=AXIS2_PLACEMENT_3D('',#11086,#7336,#7337);
#6426=AXIS2_PLACEMENT_3D('',#11088,#7338,#7339);
#6427=AXIS2_PLACEMENT_3D('',#11090,#7340,#7341);
#6428=AXIS2_PLACEMENT_3D('',#11151,#7342,#7343);
#6429=AXIS2_PLACEMENT_3D('',#11154,#7344,#7345);
#6430=AXIS2_PLACEMENT_3D('',#11172,#7347,#7348);
#6431=AXIS2_PLACEMENT_3D('',#11188,#7350,#7351);
#6432=AXIS2_PLACEMENT_3D('',#11189,#7352,#7353);
#6433=AXIS2_PLACEMENT_3D('',#11190,#7354,#7355);
#6434=AXIS2_PLACEMENT_3D('',#11191,#7356,#7357);
#6435=AXIS2_PLACEMENT_3D('',#11192,#7358,#7359);
#6436=AXIS2_PLACEMENT_3D('',#11213,#7360,#7361);
#6437=AXIS2_PLACEMENT_3D('',#11224,#7362,#7363);
#6438=AXIS2_PLACEMENT_3D('',#11235,#7364,#7365);
#6439=AXIS2_PLACEMENT_3D('',#11236,#7366,#7367);
#6440=AXIS2_PLACEMENT_3D('',#11239,#7368,#7369);
#6441=AXIS2_PLACEMENT_3D('',#11257,#7371,#7372);
#6442=AXIS2_PLACEMENT_3D('',#11273,#7374,#7375);
#6443=AXIS2_PLACEMENT_3D('',#11274,#7376,#7377);
#6444=AXIS2_PLACEMENT_3D('',#11275,#7378,#7379);
#6445=AXIS2_PLACEMENT_3D('',#11276,#7380,#7381);
#6446=AXIS2_PLACEMENT_3D('',#11277,#7382,#7383);
#6447=AXIS2_PLACEMENT_3D('',#11280,#7384,#7385);
#6448=AXIS2_PLACEMENT_3D('',#11298,#7387,#7388);
#6449=AXIS2_PLACEMENT_3D('',#11314,#7390,#7391);
#6450=AXIS2_PLACEMENT_3D('',#11315,#7392,#7393);
#6451=AXIS2_PLACEMENT_3D('',#11316,#7394,#7395);
#6452=AXIS2_PLACEMENT_3D('',#11317,#7396,#7397);
#6453=AXIS2_PLACEMENT_3D('',#11318,#7398,#7399);
#6454=AXIS2_PLACEMENT_3D('',#11321,#7400,#7401);
#6455=AXIS2_PLACEMENT_3D('',#11339,#7403,#7404);
#6456=AXIS2_PLACEMENT_3D('',#11355,#7406,#7407);
#6457=AXIS2_PLACEMENT_3D('',#11356,#7408,#7409);
#6458=AXIS2_PLACEMENT_3D('',#11357,#7410,#7411);
#6459=AXIS2_PLACEMENT_3D('',#11358,#7412,#7413);
#6460=AXIS2_PLACEMENT_3D('',#11359,#7414,#7415);
#6461=AXIS2_PLACEMENT_3D('',#11380,#7416,#7417);
#6462=AXIS2_PLACEMENT_3D('',#11391,#7418,#7419);
#6463=AXIS2_PLACEMENT_3D('',#11402,#7420,#7421);
#6464=AXIS2_PLACEMENT_3D('',#11403,#7422,#7423);
#6465=AXIS2_PLACEMENT_3D('',#11424,#7424,#7425);
#6466=AXIS2_PLACEMENT_3D('',#11435,#7426,#7427);
#6467=AXIS2_PLACEMENT_3D('',#11446,#7428,#7429);
#6468=AXIS2_PLACEMENT_3D('',#11447,#7430,#7431);
#6469=AXIS2_PLACEMENT_3D('',#11468,#7432,#7433);
#6470=AXIS2_PLACEMENT_3D('',#11479,#7434,#7435);
#6471=AXIS2_PLACEMENT_3D('',#11490,#7436,#7437);
#6472=AXIS2_PLACEMENT_3D('',#11491,#7438,#7439);
#6473=AXIS2_PLACEMENT_3D('',#11492,#7440,#7441);
#6474=AXIS2_PLACEMENT_3D('',#11493,#7442,#7443);
#6475=AXIS2_PLACEMENT_3D('',#11494,#7444,#7445);
#6476=AXIS2_PLACEMENT_3D('',#11495,#7446,#7447);
#6477=AXIS2_PLACEMENT_3D('',#11497,#7449,#7450);
#6478=AXIS2_PLACEMENT_3D('',#11498,#7451,#7452);
#6479=AXIS2_PLACEMENT_3D('',#11499,#7453,#7454);
#6480=AXIS2_PLACEMENT_3D('',#11502,#7455,#7456);
#6481=AXIS2_PLACEMENT_3D('',#11506,#7458,#7459);
#6482=AXIS2_PLACEMENT_3D('',#11508,#7461,#7462);
#6483=AXIS2_PLACEMENT_3D('',#11514,#7466,#7467);
#6484=AXIS2_PLACEMENT_3D('',#11516,#7468,#7469);
#6485=AXIS2_PLACEMENT_3D('',#11518,#7471,#7472);
#6486=AXIS2_PLACEMENT_3D('',#11522,#7475,#7476);
#6487=AXIS2_PLACEMENT_3D('',#11523,#7477,#7478);
#6488=AXIS2_PLACEMENT_3D('',#11524,#7479,#7480);
#6489=AXIS2_PLACEMENT_3D('',#11525,#7481,#7482);
#6490=AXIS2_PLACEMENT_3D('',#11528,#7483,#7484);
#6491=AXIS2_PLACEMENT_3D('',#11532,#7486,#7487);
#6492=AXIS2_PLACEMENT_3D('',#11534,#7489,#7490);
#6493=AXIS2_PLACEMENT_3D('',#11540,#7494,#7495);
#6494=AXIS2_PLACEMENT_3D('',#11542,#7496,#7497);
#6495=AXIS2_PLACEMENT_3D('',#11544,#7499,#7500);
#6496=AXIS2_PLACEMENT_3D('',#11548,#7503,#7504);
#6497=AXIS2_PLACEMENT_3D('',#11549,#7505,#7506);
#6498=AXIS2_PLACEMENT_3D('',#11550,#7507,#7508);
#6499=AXIS2_PLACEMENT_3D('',#11551,#7509,#7510);
#6500=AXIS2_PLACEMENT_3D('',#11554,#7511,#7512);
#6501=AXIS2_PLACEMENT_3D('',#11558,#7514,#7515);
#6502=AXIS2_PLACEMENT_3D('',#11560,#7517,#7518);
#6503=AXIS2_PLACEMENT_3D('',#11566,#7522,#7523);
#6504=AXIS2_PLACEMENT_3D('',#11568,#7524,#7525);
#6505=AXIS2_PLACEMENT_3D('',#11570,#7527,#7528);
#6506=AXIS2_PLACEMENT_3D('',#11574,#7531,#7532);
#6507=AXIS2_PLACEMENT_3D('',#11575,#7533,#7534);
#6508=AXIS2_PLACEMENT_3D('',#11576,#7535,#7536);
#6509=AXIS2_PLACEMENT_3D('',#11577,#7537,#7538);
#6510=AXIS2_PLACEMENT_3D('',#11582,#7540,#7541);
#6511=AXIS2_PLACEMENT_3D('',#11585,#7543,#7544);
#6512=AXIS2_PLACEMENT_3D('',#11586,#7545,#7546);
#6513=AXIS2_PLACEMENT_3D('',#11591,#7548,#7549);
#6514=AXIS2_PLACEMENT_3D('',#11594,#7551,#7552);
#6515=AXIS2_PLACEMENT_3D('',#11595,#7553,#7554);
#6516=AXIS2_PLACEMENT_3D('',#11600,#7556,#7557);
#6517=AXIS2_PLACEMENT_3D('',#11603,#7559,#7560);
#6518=AXIS2_PLACEMENT_3D('',#11604,#7561,#7562);
#6519=AXIS2_PLACEMENT_3D('',#11621,#7572,#7573);
#6520=AXIS2_PLACEMENT_3D('',#11622,#7574,#7575);
#6521=AXIS2_PLACEMENT_3D('',#11627,#7577,#7578);
#6522=AXIS2_PLACEMENT_3D('',#11630,#7580,#7581);
#6523=AXIS2_PLACEMENT_3D('',#11631,#7582,#7583);
#6524=AXIS2_PLACEMENT_3D('',#11636,#7585,#7586);
#6525=AXIS2_PLACEMENT_3D('',#11639,#7588,#7589);
#6526=AXIS2_PLACEMENT_3D('',#11640,#7590,#7591);
#6527=AXIS2_PLACEMENT_3D('',#11645,#7593,#7594);
#6528=AXIS2_PLACEMENT_3D('',#11648,#7596,#7597);
#6529=AXIS2_PLACEMENT_3D('',#11649,#7598,#7599);
#6530=AXIS2_PLACEMENT_3D('',#11666,#7609,#7610);
#6531=AXIS2_PLACEMENT_3D('',#11667,#7611,#7612);
#6532=AXIS2_PLACEMENT_3D('',#11672,#7614,#7615);
#6533=AXIS2_PLACEMENT_3D('',#11675,#7617,#7618);
#6534=AXIS2_PLACEMENT_3D('',#11676,#7619,#7620);
#6535=AXIS2_PLACEMENT_3D('',#11681,#7622,#7623);
#6536=AXIS2_PLACEMENT_3D('',#11684,#7625,#7626);
#6537=AXIS2_PLACEMENT_3D('',#11685,#7627,#7628);
#6538=AXIS2_PLACEMENT_3D('',#11690,#7630,#7631);
#6539=AXIS2_PLACEMENT_3D('',#11693,#7633,#7634);
#6540=AXIS2_PLACEMENT_3D('',#11694,#7635,#7636);
#6541=AXIS2_PLACEMENT_3D('',#11711,#7646,#7647);
#6542=AXIS2_PLACEMENT_3D('',#11712,#7648,#7649);
#6543=AXIS2_PLACEMENT_3D('',#11714,#7650,#7651);
#6544=AXIS2_PLACEMENT_3D('',#11749,#7654,#7655);
#6545=AXIS2_PLACEMENT_3D('',#11887,#7656,#7657);
#6546=AXIS2_PLACEMENT_3D('',#11889,#7658,#7659);
#6547=AXIS2_PLACEMENT_3D('',#11890,#7660,#7661);
#6548=AXIS2_PLACEMENT_3D('',#11892,#7662,#7663);
#6549=AXIS2_PLACEMENT_3D('',#11893,#7664,#7665);
#6550=AXIS2_PLACEMENT_3D('',#11895,#7666,#7667);
#6551=AXIS2_PLACEMENT_3D('',#11897,#7669,#7670);
#6552=AXIS2_PLACEMENT_3D('',#11898,#7671,#7672);
#6553=AXIS2_PLACEMENT_3D('',#11900,#7673,#7674);
#6554=AXIS2_PLACEMENT_3D('',#11902,#7676,#7677);
#6555=AXIS2_PLACEMENT_3D('',#11904,#7678,#7679);
#6556=AXIS2_PLACEMENT_3D('',#11920,#7689,#7690);
#6557=AXIS2_PLACEMENT_3D('',#11923,#7691,#7692);
#6558=AXIS2_PLACEMENT_3D('',#11924,#7693,#7694);
#6559=AXIS2_PLACEMENT_3D('',#11926,#7696,#7697);
#6560=AXIS2_PLACEMENT_3D('',#11988,#7699,#7700);
#6561=AXIS2_PLACEMENT_3D('',#11990,#7702,#7703);
#6562=AXIS2_PLACEMENT_3D('',#11992,#7704,#7705);
#6563=AXIS2_PLACEMENT_3D('',#11994,#7707,#7708);
#6564=AXIS2_PLACEMENT_3D('',#11996,#7709,#7710);
#6565=AXIS2_PLACEMENT_3D('',#11998,#7712,#7713);
#6566=AXIS2_PLACEMENT_3D('',#12000,#7714,#7715);
#6567=AXIS2_PLACEMENT_3D('',#12016,#7725,#7726);
#6568=AXIS2_PLACEMENT_3D('',#12019,#7727,#7728);
#6569=AXIS2_PLACEMENT_3D('',#12020,#7729,#7730);
#6570=AXIS2_PLACEMENT_3D('',#12022,#7732,#7733);
#6571=AXIS2_PLACEMENT_3D('',#12024,#7734,#7735);
#6572=AXIS2_PLACEMENT_3D('',#12040,#7745,#7746);
#6573=AXIS2_PLACEMENT_3D('',#12043,#7747,#7748);
#6574=AXIS2_PLACEMENT_3D('',#12044,#7749,#7750);
#6575=AXIS2_PLACEMENT_3D('',#12046,#7752,#7753);
#6576=AXIS2_PLACEMENT_3D('',#12102,#7755,#7756);
#6577=AXIS2_PLACEMENT_3D('',#12158,#7758,#7759);
#6578=AXIS2_PLACEMENT_3D('',#12160,#7761,#7762);
#6579=AXIS2_PLACEMENT_3D('',#12162,#7764,#7765);
#6580=AXIS2_PLACEMENT_3D('',#12164,#7766,#7767);
#6581=AXIS2_PLACEMENT_3D('',#12165,#7768,#7769);
#6582=AXIS2_PLACEMENT_3D('',#12168,#7772,#7773);
#6583=AXIS2_PLACEMENT_3D('',#12170,#7775,#7776);
#6584=AXIS2_PLACEMENT_3D('',#12172,#7778,#7779);
#6585=AXIS2_PLACEMENT_3D('',#12173,#7780,#7781);
#6586=AXIS2_PLACEMENT_3D('',#12175,#7783,#7784);
#6587=AXIS2_PLACEMENT_3D('',#12177,#7786,#7787);
#6588=AXIS2_PLACEMENT_3D('',#12178,#7788,#7789);
#6589=AXIS2_PLACEMENT_3D('',#12180,#7791,#7792);
#6590=AXIS2_PLACEMENT_3D('',#12182,#7794,#7795);
#6591=AXIS2_PLACEMENT_3D('',#12183,#7796,#7797);
#6592=AXIS2_PLACEMENT_3D('',#12185,#7799,#7800);
#6593=AXIS2_PLACEMENT_3D('',#12187,#7802,#7803);
#6594=AXIS2_PLACEMENT_3D('',#12188,#7804,#7805);
#6595=AXIS2_PLACEMENT_3D('',#12190,#7807,#7808);
#6596=AXIS2_PLACEMENT_3D('',#12192,#7810,#7811);
#6597=AXIS2_PLACEMENT_3D('',#12193,#7812,#7813);
#6598=AXIS2_PLACEMENT_3D('',#12195,#7815,#7816);
#6599=AXIS2_PLACEMENT_3D('',#12197,#7818,#7819);
#6600=AXIS2_PLACEMENT_3D('',#12198,#7820,#7821);
#6601=AXIS2_PLACEMENT_3D('',#12200,#7823,#7824);
#6602=AXIS2_PLACEMENT_3D('',#12202,#7826,#7827);
#6603=AXIS2_PLACEMENT_3D('',#12203,#7828,#7829);
#6604=AXIS2_PLACEMENT_3D('',#12205,#7831,#7832);
#6605=AXIS2_PLACEMENT_3D('',#12207,#7834,#7835);
#6606=AXIS2_PLACEMENT_3D('',#12208,#7836,#7837);
#6607=AXIS2_PLACEMENT_3D('',#12210,#7839,#7840);
#6608=AXIS2_PLACEMENT_3D('',#12212,#7842,#7843);
#6609=AXIS2_PLACEMENT_3D('',#12213,#7844,#7845);
#6610=AXIS2_PLACEMENT_3D('',#12214,#7846,#7847);
#6611=AXIS2_PLACEMENT_3D('',#12216,#7848,#7849);
#6612=AXIS2_PLACEMENT_3D('',#12219,#7851,#7852);
#6613=AXIS2_PLACEMENT_3D('',#12220,#7853,#7854);
#6614=AXIS2_PLACEMENT_3D('',#12222,#7855,#7856);
#6615=AXIS2_PLACEMENT_3D('',#12223,#7857,#7858);
#6616=AXIS2_PLACEMENT_3D('',#12225,#7859,#7860);
#6617=AXIS2_PLACEMENT_3D('',#12226,#7861,#7862);
#6618=AXIS2_PLACEMENT_3D('',#12228,#7863,#7864);
#6619=AXIS2_PLACEMENT_3D('',#12231,#7866,#7867);
#6620=AXIS2_PLACEMENT_3D('',#12232,#7868,#7869);
#6621=AXIS2_PLACEMENT_3D('',#12234,#7871,#7872);
#6622=AXIS2_PLACEMENT_3D('',#12236,#7873,#7874);
#6623=AXIS2_PLACEMENT_3D('',#12237,#7875,#7876);
#6624=AXIS2_PLACEMENT_3D('',#12239,#7878,#7879);
#6625=AXIS2_PLACEMENT_3D('',#12240,#7880,#7881);
#6626=AXIS2_PLACEMENT_3D('',#12242,#7882,#7883);
#6627=AXIS2_PLACEMENT_3D('',#12245,#7885,#7886);
#6628=AXIS2_PLACEMENT_3D('',#12246,#7887,#7888);
#6629=AXIS2_PLACEMENT_3D('',#12248,#7889,#7890);
#6630=AXIS2_PLACEMENT_3D('',#12249,#7891,#7892);
#6631=AXIS2_PLACEMENT_3D('',#12251,#7893,#7894);
#6632=AXIS2_PLACEMENT_3D('',#12252,#7895,#7896);
#6633=AXIS2_PLACEMENT_3D('',#12254,#7897,#7898);
#6634=AXIS2_PLACEMENT_3D('',#12257,#7900,#7901);
#6635=AXIS2_PLACEMENT_3D('',#12258,#7902,#7903);
#6636=AXIS2_PLACEMENT_3D('',#12260,#7905,#7906);
#6637=AXIS2_PLACEMENT_3D('',#12262,#7907,#7908);
#6638=AXIS2_PLACEMENT_3D('',#12263,#7909,#7910);
#6639=AXIS2_PLACEMENT_3D('',#12265,#7912,#7913);
#6640=AXIS2_PLACEMENT_3D('',#12266,#7914,#7915);
#6641=AXIS2_PLACEMENT_3D('',#12268,#7916,#7917);
#6642=AXIS2_PLACEMENT_3D('',#12271,#7919,#7920);
#6643=AXIS2_PLACEMENT_3D('',#12272,#7921,#7922);
#6644=AXIS2_PLACEMENT_3D('',#12274,#7923,#7924);
#6645=AXIS2_PLACEMENT_3D('',#12275,#7925,#7926);
#6646=AXIS2_PLACEMENT_3D('',#12277,#7927,#7928);
#6647=AXIS2_PLACEMENT_3D('',#12278,#7929,#7930);
#6648=AXIS2_PLACEMENT_3D('',#12280,#7931,#7932);
#6649=AXIS2_PLACEMENT_3D('',#12283,#7934,#7935);
#6650=AXIS2_PLACEMENT_3D('',#12284,#7936,#7937);
#6651=AXIS2_PLACEMENT_3D('',#12286,#7939,#7940);
#6652=AXIS2_PLACEMENT_3D('',#12288,#7941,#7942);
#6653=AXIS2_PLACEMENT_3D('',#12289,#7943,#7944);
#6654=AXIS2_PLACEMENT_3D('',#12291,#7946,#7947);
#6655=AXIS2_PLACEMENT_3D('',#12292,#7948,#7949);
#6656=AXIS2_PLACEMENT_3D('',#12294,#7950,#7951);
#6657=AXIS2_PLACEMENT_3D('',#12297,#7953,#7954);
#6658=AXIS2_PLACEMENT_3D('',#12298,#7955,#7956);
#6659=AXIS2_PLACEMENT_3D('',#12300,#7957,#7958);
#6660=AXIS2_PLACEMENT_3D('',#12301,#7959,#7960);
#6661=AXIS2_PLACEMENT_3D('',#12303,#7961,#7962);
#6662=AXIS2_PLACEMENT_3D('',#12304,#7963,#7964);
#6663=AXIS2_PLACEMENT_3D('',#12306,#7965,#7966);
#6664=AXIS2_PLACEMENT_3D('',#12309,#7968,#7969);
#6665=AXIS2_PLACEMENT_3D('',#12310,#7970,#7971);
#6666=AXIS2_PLACEMENT_3D('',#12312,#7973,#7974);
#6667=AXIS2_PLACEMENT_3D('',#12314,#7975,#7976);
#6668=AXIS2_PLACEMENT_3D('',#12315,#7977,#7978);
#6669=AXIS2_PLACEMENT_3D('',#12317,#7980,#7981);
#6670=AXIS2_PLACEMENT_3D('',#12318,#7982,#7983);
#6671=AXIS2_PLACEMENT_3D('',#12323,#7985,#7986);
#6672=AXIS2_PLACEMENT_3D('',#12326,#7988,#7989);
#6673=AXIS2_PLACEMENT_3D('',#12327,#7990,#7991);
#6674=AXIS2_PLACEMENT_3D('',#12332,#7993,#7994);
#6675=AXIS2_PLACEMENT_3D('',#12335,#7996,#7997);
#6676=AXIS2_PLACEMENT_3D('',#12336,#7998,#7999);
#6677=AXIS2_PLACEMENT_3D('',#12339,#8000,#8001);
#6678=AXIS2_PLACEMENT_3D('',#12343,#8003,#8004);
#6679=AXIS2_PLACEMENT_3D('',#12345,#8006,#8007);
#6680=AXIS2_PLACEMENT_3D('',#12398,#8010,#8011);
#6681=AXIS2_PLACEMENT_3D('',#12444,#8014,#8015);
#6682=AXIS2_PLACEMENT_3D('',#12490,#8018,#8019);
#6683=AXIS2_PLACEMENT_3D('',#12543,#8022,#8023);
#6684=AXIS2_PLACEMENT_3D('',#12546,#8024,#8025);
#6685=AXIS2_PLACEMENT_3D('',#12550,#8027,#8028);
#6686=AXIS2_PLACEMENT_3D('',#12552,#8030,#8031);
#6687=AXIS2_PLACEMENT_3D('',#12605,#8034,#8035);
#6688=AXIS2_PLACEMENT_3D('',#12651,#8038,#8039);
#6689=AXIS2_PLACEMENT_3D('',#12697,#8042,#8043);
#6690=AXIS2_PLACEMENT_3D('',#12750,#8046,#8047);
#6691=AXIS2_PLACEMENT_3D('',#12803,#8050,#8051);
#6692=AXIS2_PLACEMENT_3D('',#12849,#8054,#8055);
#6693=AXIS2_PLACEMENT_3D('',#12895,#8058,#8059);
#6694=AXIS2_PLACEMENT_3D('',#12948,#8062,#8063);
#6695=AXIS2_PLACEMENT_3D('',#12951,#8064,#8065);
#6696=AXIS2_PLACEMENT_3D('',#12955,#8067,#8068);
#6697=AXIS2_PLACEMENT_3D('',#12957,#8070,#8071);
#6698=AXIS2_PLACEMENT_3D('',#12962,#8073,#8074);
#6699=AXIS2_PLACEMENT_3D('',#12965,#8076,#8077);
#6700=AXIS2_PLACEMENT_3D('',#12966,#8078,#8079);
#6701=AXIS2_PLACEMENT_3D('',#12968,#8080,#8081);
#6702=AXIS2_PLACEMENT_3D('',#12972,#8083,#8084);
#6703=AXIS2_PLACEMENT_3D('',#12977,#8087,#8088);
#6704=AXIS2_PLACEMENT_3D('',#12982,#8091,#8092);
#6705=AXIS2_PLACEMENT_3D('',#12984,#8094,#8095);
#6706=AXIS2_PLACEMENT_3D('',#12986,#8096,#8097);
#6707=AXIS2_PLACEMENT_3D('',#13002,#8107,#8108);
#6708=AXIS2_PLACEMENT_3D('',#13004,#8110,#8111);
#6709=AXIS2_PLACEMENT_3D('',#13021,#8121,#8122);
#6710=AXIS2_PLACEMENT_3D('',#13022,#8123,#8124);
#6711=AXIS2_PLACEMENT_3D('',#13026,#8126,#8127);
#6712=AXIS2_PLACEMENT_3D('',#13031,#8130,#8131);
#6713=AXIS2_PLACEMENT_3D('',#13036,#8134,#8135);
#6714=AXIS2_PLACEMENT_3D('',#13038,#8137,#8138);
#6715=AXIS2_PLACEMENT_3D('',#13040,#8139,#8140);
#6716=AXIS2_PLACEMENT_3D('',#13042,#8141,#8142);
#6717=AXIS2_PLACEMENT_3D('',#13043,#8143,#8144);
#6718=AXIS2_PLACEMENT_3D('',#13067,#8148,#8149);
#6719=AXIS2_PLACEMENT_3D('',#13069,#8150,#8151);
#6720=AXIS2_PLACEMENT_3D('',#13071,#8152,#8153);
#6721=AXIS2_PLACEMENT_3D('',#13072,#8154,#8155);
#6722=AXIS2_PLACEMENT_3D('',#13074,#8157,#8158);
#6723=AXIS2_PLACEMENT_3D('',#13076,#8159,#8160);
#6724=AXIS2_PLACEMENT_3D('',#13078,#8161,#8162);
#6725=AXIS2_PLACEMENT_3D('',#13079,#8163,#8164);
#6726=AXIS2_PLACEMENT_3D('',#13081,#8166,#8167);
#6727=AXIS2_PLACEMENT_3D('',#13083,#8168,#8169);
#6728=AXIS2_PLACEMENT_3D('',#13085,#8170,#8171);
#6729=AXIS2_PLACEMENT_3D('',#13086,#8172,#8173);
#6730=AXIS2_PLACEMENT_3D('',#13088,#8175,#8176);
#6731=AXIS2_PLACEMENT_3D('',#13090,#8177,#8178);
#6732=AXIS2_PLACEMENT_3D('',#13092,#8179,#8180);
#6733=AXIS2_PLACEMENT_3D('',#13093,#8181,#8182);
#6734=AXIS2_PLACEMENT_3D('',#13095,#8184,#8185);
#6735=AXIS2_PLACEMENT_3D('',#13097,#8186,#8187);
#6736=AXIS2_PLACEMENT_3D('',#13099,#8188,#8189);
#6737=AXIS2_PLACEMENT_3D('',#13100,#8190,#8191);
#6738=AXIS2_PLACEMENT_3D('',#13102,#8193,#8194);
#6739=AXIS2_PLACEMENT_3D('',#13104,#8195,#8196);
#6740=AXIS2_PLACEMENT_3D('',#13106,#8197,#8198);
#6741=AXIS2_PLACEMENT_3D('',#13107,#8199,#8200);
#6742=AXIS2_PLACEMENT_3D('',#13109,#8202,#8203);
#6743=AXIS2_PLACEMENT_3D('',#13111,#8204,#8205);
#6744=AXIS2_PLACEMENT_3D('',#13641,#8207,#8208);
#6745=AXIS2_PLACEMENT_3D('',#13642,#8209,#8210);
#6746=AXIS2_PLACEMENT_3D('',#13644,#8211,#8212);
#6747=AXIS2_PLACEMENT_3D('',#13646,#8213,#8214);
#6748=AXIS2_PLACEMENT_3D('',#13647,#8215,#8216);
#6749=AXIS2_PLACEMENT_3D('',#13649,#8218,#8219);
#6750=AXIS2_PLACEMENT_3D('',#13651,#8221,#8222);
#6751=AXIS2_PLACEMENT_3D('',#13653,#8224,#8225);
#6752=AXIS2_PLACEMENT_3D('',#13655,#8227,#8228);
#6753=AXIS2_PLACEMENT_3D('',#13657,#8230,#8231);
#6754=AXIS2_PLACEMENT_3D('',#13659,#8232,#8233);
#6755=AXIS2_PLACEMENT_3D('',#13661,#8234,#8235);
#6756=AXIS2_PLACEMENT_3D('',#13662,#8236,#8237);
#6757=AXIS2_PLACEMENT_3D('',#13686,#8241,#8242);
#6758=AXIS2_PLACEMENT_3D('',#13688,#8243,#8244);
#6759=AXIS2_PLACEMENT_3D('',#13690,#8245,#8246);
#6760=AXIS2_PLACEMENT_3D('',#13691,#8247,#8248);
#6761=AXIS2_PLACEMENT_3D('',#13715,#8252,#8253);
#6762=AXIS2_PLACEMENT_3D('',#13717,#8254,#8255);
#6763=AXIS2_PLACEMENT_3D('',#13719,#8256,#8257);
#6764=AXIS2_PLACEMENT_3D('',#13720,#8258,#8259);
#6765=AXIS2_PLACEMENT_3D('',#13722,#8261,#8262);
#6766=AXIS2_PLACEMENT_3D('',#13724,#8263,#8264);
#6767=AXIS2_PLACEMENT_3D('',#13726,#8265,#8266);
#6768=AXIS2_PLACEMENT_3D('',#13727,#8267,#8268);
#6769=AXIS2_PLACEMENT_3D('',#13729,#8270,#8271);
#6770=AXIS2_PLACEMENT_3D('',#13731,#8272,#8273);
#6771=AXIS2_PLACEMENT_3D('',#13733,#8274,#8275);
#6772=AXIS2_PLACEMENT_3D('',#13734,#8276,#8277);
#6773=AXIS2_PLACEMENT_3D('',#13736,#8279,#8280);
#6774=AXIS2_PLACEMENT_3D('',#13738,#8281,#8282);
#6775=AXIS2_PLACEMENT_3D('',#13740,#8283,#8284);
#6776=AXIS2_PLACEMENT_3D('',#13741,#8285,#8286);
#6777=AXIS2_PLACEMENT_3D('',#13743,#8288,#8289);
#6778=AXIS2_PLACEMENT_3D('',#13745,#8290,#8291);
#6779=AXIS2_PLACEMENT_3D('',#13747,#8292,#8293);
#6780=AXIS2_PLACEMENT_3D('',#13748,#8294,#8295);
#6781=AXIS2_PLACEMENT_3D('',#13750,#8297,#8298);
#6782=AXIS2_PLACEMENT_3D('',#13752,#8299,#8300);
#6783=AXIS2_PLACEMENT_3D('',#13754,#8301,#8302);
#6784=AXIS2_PLACEMENT_3D('',#13755,#8303,#8304);
#6785=AXIS2_PLACEMENT_3D('',#13757,#8306,#8307);
#6786=AXIS2_PLACEMENT_3D('',#13760,#8309,#8310);
#6787=AXIS2_PLACEMENT_3D('',#13761,#8311,#8312);
#6788=AXIS2_PLACEMENT_3D('',#13764,#8314,#8315);
#6789=AXIS2_PLACEMENT_3D('',#13765,#8316,#8317);
#6790=AXIS2_PLACEMENT_3D('',#13768,#8319,#8320);
#6791=AXIS2_PLACEMENT_3D('',#13769,#8321,#8322);
#6792=AXIS2_PLACEMENT_3D('',#13772,#8324,#8325);
#6793=AXIS2_PLACEMENT_3D('',#13773,#8326,#8327);
#6794=AXIS2_PLACEMENT_3D('',#13776,#8329,#8330);
#6795=AXIS2_PLACEMENT_3D('',#13777,#8331,#8332);
#6796=AXIS2_PLACEMENT_3D('',#13780,#8334,#8335);
#6797=AXIS2_PLACEMENT_3D('',#13781,#8336,#8337);
#6798=AXIS2_PLACEMENT_3D('',#13784,#8339,#8340);
#6799=AXIS2_PLACEMENT_3D('',#13785,#8341,#8342);
#6800=AXIS2_PLACEMENT_3D('',#13788,#8344,#8345);
#6801=AXIS2_PLACEMENT_3D('',#13789,#8346,#8347);
#6802=AXIS2_PLACEMENT_3D('',#13791,#8348,#8349);
#6803=AXIS2_PLACEMENT_3D('',#13792,#8350,#8351);
#6804=AXIS2_PLACEMENT_3D('',#13794,#8353,#8354);
#6805=AXIS2_PLACEMENT_3D('',#13796,#8355,#8356);
#6806=AXIS2_PLACEMENT_3D('',#13797,#8357,#8358);
#6807=AXIS2_PLACEMENT_3D('',#13799,#8360,#8361);
#6808=AXIS2_PLACEMENT_3D('',#13801,#8362,#8363);
#6809=AXIS2_PLACEMENT_3D('',#13802,#8364,#8365);
#6810=AXIS2_PLACEMENT_3D('',#13804,#8367,#8368);
#6811=AXIS2_PLACEMENT_3D('',#13806,#8369,#8370);
#6812=AXIS2_PLACEMENT_3D('',#13807,#8371,#8372);
#6813=AXIS2_PLACEMENT_3D('',#13809,#8374,#8375);
#6814=AXIS2_PLACEMENT_3D('',#13811,#8376,#8377);
#6815=AXIS2_PLACEMENT_3D('',#13812,#8378,#8379);
#6816=AXIS2_PLACEMENT_3D('',#13814,#8381,#8382);
#6817=AXIS2_PLACEMENT_3D('',#13816,#8383,#8384);
#6818=AXIS2_PLACEMENT_3D('',#13817,#8385,#8386);
#6819=AXIS2_PLACEMENT_3D('',#13819,#8388,#8389);
#6820=AXIS2_PLACEMENT_3D('',#13821,#8390,#8391);
#6821=AXIS2_PLACEMENT_3D('',#13822,#8392,#8393);
#6822=AXIS2_PLACEMENT_3D('',#13824,#8395,#8396);
#6823=AXIS2_PLACEMENT_3D('',#13826,#8397,#8398);
#6824=AXIS2_PLACEMENT_3D('',#13827,#8399,#8400);
#6825=AXIS2_PLACEMENT_3D('',#13829,#8402,#8403);
#6826=AXIS2_PLACEMENT_3D('',#13831,#8405,#8406);
#6827=AXIS2_PLACEMENT_3D('',#13833,#8408,#8409);
#6828=AXIS2_PLACEMENT_3D('',#13837,#8412,#8413);
#6829=AXIS2_PLACEMENT_3D('',#13891,#8416,#8417);
#6830=AXIS2_PLACEMENT_3D('',#13892,#8418,#8419);
#6831=AXIS2_PLACEMENT_3D('',#13894,#8421,#8422);
#6832=AXIS2_PLACEMENT_3D('',#13896,#8424,#8425);
#6833=AXIS2_PLACEMENT_3D('',#13900,#8428,#8429);
#6834=AXIS2_PLACEMENT_3D('',#13954,#8432,#8433);
#6835=AXIS2_PLACEMENT_3D('',#13955,#8434,#8435);
#6836=AXIS2_PLACEMENT_3D('',#13957,#8437,#8438);
#6837=AXIS2_PLACEMENT_3D('',#13959,#8440,#8441);
#6838=AXIS2_PLACEMENT_3D('',#13963,#8444,#8445);
#6839=AXIS2_PLACEMENT_3D('',#14017,#8448,#8449);
#6840=AXIS2_PLACEMENT_3D('',#14018,#8450,#8451);
#6841=AXIS2_PLACEMENT_3D('',#14020,#8453,#8454);
#6842=AXIS2_PLACEMENT_3D('',#14022,#8456,#8457);
#6843=AXIS2_PLACEMENT_3D('',#14023,#8458,#8459);
#6844=AXIS2_PLACEMENT_3D('',#14025,#8461,#8462);
#6845=AXIS2_PLACEMENT_3D('',#14027,#8464,#8465);
#6846=AXIS2_PLACEMENT_3D('',#14028,#8466,#8467);
#6847=AXIS2_PLACEMENT_3D('',#14030,#8469,#8470);
#6848=AXIS2_PLACEMENT_3D('',#14032,#8472,#8473);
#6849=AXIS2_PLACEMENT_3D('',#14033,#8474,#8475);
#6850=AXIS2_PLACEMENT_3D('',#14034,#8476,#8477);
#6851=AXIS2_PLACEMENT_3D('',#14035,#8478,#8479);
#6852=AXIS2_PLACEMENT_3D('',#14036,#8480,#8481);
#6853=AXIS2_PLACEMENT_3D('',#14037,#8482,#8483);
#6854=AXIS2_PLACEMENT_3D('',#14038,#8484,#8485);
#6855=AXIS2_PLACEMENT_3D('',#14039,#8486,#8487);
#6856=AXIS2_PLACEMENT_3D('',#14040,#8488,#8489);
#6857=AXIS2_PLACEMENT_3D('',#14041,#8490,#8491);
#6858=AXIS2_PLACEMENT_3D('',#14042,#8492,#8493);
#6859=AXIS2_PLACEMENT_3D('',#14043,#8494,#8495);
#6860=AXIS2_PLACEMENT_3D('',#14044,#8496,#8497);
#6861=AXIS2_PLACEMENT_3D('',#14045,#8498,#8499);
#6862=AXIS2_PLACEMENT_3D('',#14046,#8500,#8501);
#6863=AXIS2_PLACEMENT_3D('',#14047,#8502,#8503);
#6864=AXIS2_PLACEMENT_3D('',#14048,#8504,#8505);
#6865=AXIS2_PLACEMENT_3D('',#14049,#8506,#8507);
#6866=AXIS2_PLACEMENT_3D('',#14050,#8508,#8509);
#6867=AXIS2_PLACEMENT_3D('',#14051,#8510,#8511);
#6868=AXIS2_PLACEMENT_3D('',#14052,#8512,#8513);
#6869=AXIS2_PLACEMENT_3D('',#14053,#8514,#8515);
#6870=AXIS2_PLACEMENT_3D('',#14054,#8516,#8517);
#6871=AXIS2_PLACEMENT_3D('',#14055,#8518,#8519);
#6872=AXIS2_PLACEMENT_3D('',#14056,#8520,#8521);
#6873=AXIS2_PLACEMENT_3D('',#14057,#8522,#8523);
#6874=AXIS2_PLACEMENT_3D('',#14058,#8524,#8525);
#6875=AXIS2_PLACEMENT_3D('',#14059,#8526,#8527);
#6876=AXIS2_PLACEMENT_3D('',#14060,#8528,#8529);
#6877=AXIS2_PLACEMENT_3D('',#14061,#8530,#8531);
#6878=AXIS2_PLACEMENT_3D('',#14062,#8532,#8533);
#6879=AXIS2_PLACEMENT_3D('',#14063,#8534,#8535);
#6880=AXIS2_PLACEMENT_3D('',#14064,#8536,#8537);
#6881=AXIS2_PLACEMENT_3D('',#14065,#8538,#8539);
#6882=AXIS2_PLACEMENT_3D('',#14066,#8540,#8541);
#6883=AXIS2_PLACEMENT_3D('',#14067,#8542,#8543);
#6884=AXIS2_PLACEMENT_3D('',#14068,#8544,#8545);
#6885=AXIS2_PLACEMENT_3D('',#14069,#8546,#8547);
#6886=AXIS2_PLACEMENT_3D('',#14070,#8548,#8549);
#6887=AXIS2_PLACEMENT_3D('',#14071,#8550,#8551);
#6888=AXIS2_PLACEMENT_3D('',#14072,#8552,#8553);
#6889=AXIS2_PLACEMENT_3D('',#14073,#8554,#8555);
#6890=AXIS2_PLACEMENT_3D('',#14074,#8556,#8557);
#6891=AXIS2_PLACEMENT_3D('',#14076,#8558,#8559);
#6892=AXIS2_PLACEMENT_3D('',#14079,#8561,#8562);
#6893=AXIS2_PLACEMENT_3D('',#14080,#8563,#8564);
#6894=AXIS2_PLACEMENT_3D('',#14082,#8565,#8566);
#6895=AXIS2_PLACEMENT_3D('',#14083,#8567,#8568);
#6896=AXIS2_PLACEMENT_3D('',#14085,#8569,#8570);
#6897=AXIS2_PLACEMENT_3D('',#14086,#8571,#8572);
#6898=AXIS2_PLACEMENT_3D('',#14089,#8574,#8575);
#6899=AXIS2_PLACEMENT_3D('',#14090,#8576,#8577);
#6900=AXIS2_PLACEMENT_3D('',#14092,#8578,#8579);
#6901=AXIS2_PLACEMENT_3D('',#14093,#8580,#8581);
#6902=AXIS2_PLACEMENT_3D('',#14095,#8583,#8584);
#6903=AXIS2_PLACEMENT_3D('',#14096,#8585,#8586);
#6904=AXIS2_PLACEMENT_3D('',#14097,#8587,#8588);
#6905=AXIS2_PLACEMENT_3D('',#14098,#8589,#8590);
#6906=AXIS2_PLACEMENT_3D('',#14099,#8591,#8592);
#6907=DIRECTION('axis',(0.,0.,1.));
#6908=DIRECTION('refdir',(1.,0.,0.));
#6909=DIRECTION('axis',(0.,0.,1.));
#6910=DIRECTION('refdir',(1.,0.,0.));
#6911=DIRECTION('center_axis',(0.,1.,0.));
#6912=DIRECTION('ref_axis',(0.,0.,1.));
#6913=DIRECTION('',(1.,0.,-1.4799935157375E-16));
#6914=DIRECTION('',(0.,0.,-1.));
#6915=DIRECTION('',(1.,0.,-1.47999351573749E-16));
#6916=DIRECTION('',(0.,3.88578058618804E-16,-1.));
#6917=DIRECTION('',(-1.,0.,0.));
#6918=DIRECTION('center_axis',(0.,1.,0.));
#6919=DIRECTION('ref_axis',(0.,0.,1.));
#6920=DIRECTION('',(1.,0.,-4.40139925476306E-16));
#6921=DIRECTION('',(0.,0.,1.));
#6922=DIRECTION('center_axis',(0.,1.,0.));
#6923=DIRECTION('ref_axis',(0.,0.,-1.));
#6924=DIRECTION('center_axis',(0.,1.,0.));
#6925=DIRECTION('ref_axis',(0.,0.,1.));
#6926=DIRECTION('center_axis',(0.,1.,0.));
#6927=DIRECTION('ref_axis',(0.,0.,1.));
#6928=DIRECTION('center_axis',(0.,-1.,0.));
#6929=DIRECTION('ref_axis',(0.,0.,-1.));
#6930=DIRECTION('center_axis',(-7.86509422263479E-32,-1.,-4.2478565844662E-16));
#6931=DIRECTION('ref_axis',(-3.70308840058128E-16,4.24785658446619E-16,
-1.));
#6932=DIRECTION('center_axis',(0.,1.,0.));
#6933=DIRECTION('ref_axis',(0.,0.,-1.));
#6934=DIRECTION('center_axis',(0.,1.,0.));
#6935=DIRECTION('ref_axis',(0.,0.,1.));
#6936=DIRECTION('center_axis',(0.,1.,0.));
#6937=DIRECTION('ref_axis',(0.,0.,1.));
#6938=DIRECTION('center_axis',(0.,-1.,0.));
#6939=DIRECTION('ref_axis',(0.,0.,-1.));
#6940=DIRECTION('center_axis',(0.,1.,0.));
#6941=DIRECTION('ref_axis',(0.,0.,1.));
#6942=DIRECTION('center_axis',(7.86509422263479E-32,1.,4.2478565844662E-16));
#6943=DIRECTION('ref_axis',(3.70308840058128E-16,-4.2478565844662E-16,1.));
#6944=DIRECTION('center_axis',(-7.86509422263479E-32,-1.,-4.2478565844662E-16));
#6945=DIRECTION('ref_axis',(-3.70308840058128E-16,4.24785658446619E-16,
-1.));
#6946=DIRECTION('',(-2.10042193848003E-16,0.,1.));
#6947=DIRECTION('',(1.,0.,3.88971843979164E-16));
#6948=DIRECTION('',(0.,0.,-1.));
#6949=DIRECTION('',(-1.,0.,0.));
#6950=DIRECTION('center_axis',(0.,-1.,0.));
#6951=DIRECTION('ref_axis',(0.,0.,-1.));
#6952=DIRECTION('center_axis',(0.,-1.,0.));
#6953=DIRECTION('ref_axis',(0.,0.,-1.));
#6954=DIRECTION('center_axis',(0.,-1.,0.));
#6955=DIRECTION('ref_axis',(0.,0.,-1.));
#6956=DIRECTION('center_axis',(0.,-1.,0.));
#6957=DIRECTION('ref_axis',(0.,0.,-1.));
#6958=DIRECTION('center_axis',(0.,-1.,0.));
#6959=DIRECTION('ref_axis',(0.,0.,-1.));
#6960=DIRECTION('center_axis',(0.,-1.,0.));
#6961=DIRECTION('ref_axis',(0.,0.,-1.));
#6962=DIRECTION('',(-1.,0.,3.88971843979164E-16));
#6963=DIRECTION('',(2.10042193848003E-16,0.,1.));
#6964=DIRECTION('',(1.,0.,0.));
#6965=DIRECTION('',(0.,0.,-1.));
#6966=DIRECTION('center_axis',(0.,1.,0.));
#6967=DIRECTION('ref_axis',(0.,0.,1.));
#6968=DIRECTION('center_axis',(0.,-1.,0.));
#6969=DIRECTION('ref_axis',(0.,0.,-1.));
#6970=DIRECTION('',(0.,1.,0.));
#6971=DIRECTION('center_axis',(0.,1.,0.));
#6972=DIRECTION('ref_axis',(0.,0.,1.));
#6973=DIRECTION('center_axis',(-1.,1.4811191380744E-16,1.85154420029064E-16));
#6974=DIRECTION('ref_axis',(1.85154420029064E-16,0.,1.));
#6975=DIRECTION('center_axis',(1.,1.4811191380744E-16,1.85154420029064E-16));
#6976=DIRECTION('ref_axis',(1.85154420029064E-16,0.,-1.));
#6977=DIRECTION('',(-1.,1.4811191380744E-16,1.85154420029064E-16));
#6978=DIRECTION('center_axis',(2.37862219570569E-17,0.,1.));
#6979=DIRECTION('ref_axis',(1.,0.,-2.37862219570569E-17));
#6980=DIRECTION('',(1.20024110770287E-16,-4.80096443081149E-16,1.));
#6981=DIRECTION('',(2.40048221540575E-16,-4.80096443081149E-16,1.));
#6982=DIRECTION('center_axis',(-3.46522618101071E-16,4.2478565844662E-16,
-1.));
#6983=DIRECTION('ref_axis',(-1.,-6.8546896270362E-32,3.46522618101071E-16));
#6984=DIRECTION('',(0.,0.,-1.));
#6985=DIRECTION('',(0.,0.,-1.));
#6986=DIRECTION('center_axis',(-3.46522618101071E-16,4.2478565844662E-16,
-1.));
#6987=DIRECTION('ref_axis',(-1.,-6.8546896270362E-32,3.46522618101071E-16));
#6988=DIRECTION('center_axis',(0.,1.,0.));
#6989=DIRECTION('ref_axis',(0.,0.,1.));
#6990=DIRECTION('',(0.,0.,-1.));
#6991=DIRECTION('',(1.,0.,-1.47999270653708E-16));
#6992=DIRECTION('',(0.,0.,1.));
#6993=DIRECTION('',(1.,0.,0.));
#6994=DIRECTION('center_axis',(0.,1.,0.));
#6995=DIRECTION('ref_axis',(0.,0.,-1.));
#6996=DIRECTION('',(-1.,0.,4.40139925486788E-16));
#6997=DIRECTION('',(0.,3.88578058618805E-16,-1.));
#6998=DIRECTION('',(1.,0.,-2.95998541307373E-16));
#6999=DIRECTION('center_axis',(0.,-1.,0.));
#7000=DIRECTION('ref_axis',(0.,0.,-1.));
#7001=DIRECTION('center_axis',(0.,-1.,0.));
#7002=DIRECTION('ref_axis',(0.,0.,1.));
#7003=DIRECTION('center_axis',(0.,-1.,0.));
#7004=DIRECTION('ref_axis',(0.,0.,1.));
#7005=DIRECTION('center_axis',(-1.85154420029064E-16,2.1239282922331E-16,
-1.));
#7006=DIRECTION('ref_axis',(-1.,0.,1.85154420029064E-16));
#7007=DIRECTION('center_axis',(-2.37862219570569E-17,0.,-1.));
#7008=DIRECTION('ref_axis',(-1.,0.,2.37862219570569E-17));
#7009=DIRECTION('',(2.30359800135544E-16,1.,1.72769850101658E-16));
#7010=DIRECTION('',(0.,1.,0.));
#7011=DIRECTION('center_axis',(-1.85154420029064E-16,2.1239282922331E-16,
-1.));
#7012=DIRECTION('ref_axis',(-1.,0.,1.85154420029064E-16));
#7013=DIRECTION('',(0.,1.,0.));
#7014=DIRECTION('',(-5.7589950033886E-17,-1.,-2.30359800135544E-16));
#7015=DIRECTION('center_axis',(-2.37862219570569E-17,0.,-1.));
#7016=DIRECTION('ref_axis',(-1.,0.,2.37862219570569E-17));
#7017=DIRECTION('center_axis',(1.85154420029064E-16,-2.1239282922331E-16,
1.));
#7018=DIRECTION('ref_axis',(1.,0.,-1.85154420029064E-16));
#7019=DIRECTION('',(0.,1.,0.));
#7020=DIRECTION('',(-2.30359800135544E-16,-1.,-1.15179900067772E-16));
#7021=DIRECTION('center_axis',(1.85154420029064E-16,-2.1239282922331E-16,
1.));
#7022=DIRECTION('ref_axis',(1.,0.,-1.85154420029064E-16));
#7023=DIRECTION('',(2.8794975016943E-17,1.,2.30359800135544E-16));
#7024=DIRECTION('',(0.,1.,0.));
#7025=DIRECTION('center_axis',(-6.3741727053016E-17,0.,-1.));
#7026=DIRECTION('ref_axis',(-1.,0.,6.3741727053016E-17));
#7027=DIRECTION('',(0.,1.,0.));
#7028=DIRECTION('center_axis',(-6.3741727053016E-17,0.,-1.));
#7029=DIRECTION('ref_axis',(-1.,0.,6.3741727053016E-17));
#7030=DIRECTION('',(0.,1.,0.));
#7031=DIRECTION('center_axis',(0.,1.,0.));
#7032=DIRECTION('ref_axis',(0.,0.,1.));
#7033=DIRECTION('',(0.,1.,0.));
#7034=DIRECTION('',(0.,1.,0.));
#7035=DIRECTION('center_axis',(0.,1.,0.));
#7036=DIRECTION('ref_axis',(0.,0.,1.));
#7037=DIRECTION('',(0.,1.,0.));
#7038=DIRECTION('',(0.,1.,0.));
#7039=DIRECTION('center_axis',(0.,1.,0.));
#7040=DIRECTION('ref_axis',(0.,0.,1.));
#7041=DIRECTION('',(-0.00148924434041068,-0.517944475025485,0.855412942935673));
#7042=DIRECTION('',(-0.0014892443404113,0.517944475025485,-0.855412942935673));
#7043=DIRECTION('',(0.,0.,1.));
#7044=DIRECTION('center_axis',(2.37862219570569E-17,0.,1.));
#7045=DIRECTION('ref_axis',(1.,0.,-2.37862219570569E-17));
#7046=DIRECTION('',(1.80036166155431E-16,0.,1.));
#7047=DIRECTION('',(2.40048221540574E-16,0.,1.));
#7048=DIRECTION('',(0.,0.,1.));
#7049=DIRECTION('center_axis',(6.3741727053016E-17,0.,1.));
#7050=DIRECTION('ref_axis',(1.,0.,-6.3741727053016E-17));
#7051=DIRECTION('',(0.,1.,0.));
#7052=DIRECTION('center_axis',(6.3741727053016E-17,0.,1.));
#7053=DIRECTION('ref_axis',(1.,0.,-6.3741727053016E-17));
#7054=DIRECTION('',(0.,1.,0.));
#7055=DIRECTION('center_axis',(0.,1.,0.));
#7056=DIRECTION('ref_axis',(0.,0.,1.));
#7057=DIRECTION('',(0.,1.,0.));
#7058=DIRECTION('center_axis',(0.,1.,0.));
#7059=DIRECTION('ref_axis',(0.,0.,1.));
#7060=DIRECTION('',(0.,1.,0.));
#7061=DIRECTION('center_axis',(7.86509422263479E-32,1.,4.2478565844662E-16));
#7062=DIRECTION('ref_axis',(-3.70308840058128E-16,4.2478565844662E-16,-1.));
#7063=DIRECTION('',(0.,1.,0.));
#7064=DIRECTION('center_axis',(7.86509422263479E-32,1.,4.2478565844662E-16));
#7065=DIRECTION('ref_axis',(-3.70308840058128E-16,4.24785658446619E-16,
-1.));
#7066=DIRECTION('',(0.,1.,0.));
#7067=DIRECTION('center_axis',(7.86509422263479E-32,1.,4.2478565844662E-16));
#7068=DIRECTION('ref_axis',(-3.70308840058128E-16,4.24785658446619E-16,
-1.));
#7069=DIRECTION('',(-0.00148924434041153,-0.517944475025485,-0.855412942935673));
#7070=DIRECTION('',(-0.00148924434041087,0.517944475025484,0.855412942935674));
#7071=DIRECTION('center_axis',(1.,-2.06784640888072E-16,-1.85154420029064E-16));
#7072=DIRECTION('ref_axis',(-1.85154420029064E-16,0.,-1.));
#7073=DIRECTION('center_axis',(-1.,1.4811191380744E-16,1.85154420029064E-16));
#7074=DIRECTION('ref_axis',(1.85154420029064E-16,0.,1.));
#7075=DIRECTION('center_axis',(-1.,1.4811191380744E-16,1.85154420029064E-16));
#7076=DIRECTION('ref_axis',(1.85154420029064E-16,0.,1.));
#7077=DIRECTION('center_axis',(-1.,5.16961602220179E-17,1.85154420029064E-16));
#7078=DIRECTION('ref_axis',(1.85154420029064E-16,0.,1.));
#7079=DIRECTION('center_axis',(-1.,-1.4811191380744E-16,-1.85154420029064E-16));
#7080=DIRECTION('ref_axis',(-1.85154420029064E-16,0.,1.));
#7081=DIRECTION('center_axis',(-1.,-1.4811191380744E-16,-1.85154420029064E-16));
#7082=DIRECTION('ref_axis',(-1.85154420029064E-16,0.,1.));
#7083=DIRECTION('center_axis',(1.,-1.4811191380744E-16,-1.85154420029064E-16));
#7084=DIRECTION('ref_axis',(-1.85154420029064E-16,0.,-1.));
#7085=DIRECTION('',(-1.,1.4811191380744E-16,1.85154420029064E-16));
#7086=DIRECTION('center_axis',(-1.,1.4811191380744E-16,1.85154420029064E-16));
#7087=DIRECTION('ref_axis',(1.85154420029064E-16,0.,1.));
#7088=DIRECTION('center_axis',(-1.,1.4811191380744E-16,1.85154420029064E-16));
#7089=DIRECTION('ref_axis',(1.85154420029064E-16,0.,1.));
#7090=DIRECTION('center_axis',(-1.,1.4811191380744E-16,1.85154420029064E-16));
#7091=DIRECTION('ref_axis',(1.85154420029064E-16,0.,1.));
#7092=DIRECTION('center_axis',(-1.,-1.4811191380744E-16,-1.85154420029064E-16));
#7093=DIRECTION('ref_axis',(-1.85154420029064E-16,0.,1.));
#7094=DIRECTION('',(1.,1.4811191380744E-16,1.85154420029064E-16));
#7095=DIRECTION('center_axis',(-1.,-1.4811191380744E-16,-1.85154420029064E-16));
#7096=DIRECTION('ref_axis',(-1.85154420029064E-16,0.,1.));
#7097=DIRECTION('center_axis',(1.,1.4811191380744E-16,1.85154420029064E-16));
#7098=DIRECTION('ref_axis',(1.85154420029064E-16,0.,-1.));
#7099=DIRECTION('center_axis',(-1.,1.4811191380744E-16,1.85154420029064E-16));
#7100=DIRECTION('ref_axis',(1.85154420029064E-16,0.,1.));
#7101=DIRECTION('',(-1.,1.4811191380744E-16,1.85154420029064E-16));
#7102=DIRECTION('center_axis',(0.,1.,0.));
#7103=DIRECTION('ref_axis',(0.,0.,1.));
#7104=DIRECTION('center_axis',(0.,1.,0.));
#7105=DIRECTION('ref_axis',(0.,0.,1.));
#7106=DIRECTION('center_axis',(0.,1.,0.));
#7107=DIRECTION('ref_axis',(0.,0.,1.));
#7108=DIRECTION('',(0.,-1.,0.));
#7109=DIRECTION('center_axis',(0.,-1.,0.));
#7110=DIRECTION('ref_axis',(0.,0.,-1.));
#7111=DIRECTION('center_axis',(1.,0.,0.));
#7112=DIRECTION('ref_axis',(0.,0.,-1.));
#7113=DIRECTION('center_axis',(1.,0.,0.));
#7114=DIRECTION('ref_axis',(0.,0.,-1.));
#7115=DIRECTION('center_axis',(0.,1.,0.));
#7116=DIRECTION('ref_axis',(0.,0.,1.));
#7117=DIRECTION('',(0.,1.,0.));
#7118=DIRECTION('center_axis',(0.,1.,0.));
#7119=DIRECTION('ref_axis',(0.,0.,1.));
#7120=DIRECTION('',(0.,1.,0.));
#7121=DIRECTION('center_axis',(0.,1.,0.));
#7122=DIRECTION('ref_axis',(0.,0.,1.));
#7123=DIRECTION('',(0.,1.,0.));
#7124=DIRECTION('center_axis',(0.,1.,0.));
#7125=DIRECTION('ref_axis',(0.,0.,1.));
#7126=DIRECTION('',(0.,1.,0.));
#7127=DIRECTION('center_axis',(0.,1.,0.));
#7128=DIRECTION('ref_axis',(0.,0.,1.));
#7129=DIRECTION('',(0.,1.,0.));
#7130=DIRECTION('center_axis',(0.,1.,0.));
#7131=DIRECTION('ref_axis',(0.,0.,1.));
#7132=DIRECTION('',(0.,1.,0.));
#7133=DIRECTION('axis',(0.,0.,1.));
#7134=DIRECTION('refdir',(1.,0.,0.));
#7135=DIRECTION('center_axis',(-1.,-1.4811191380744E-16,-1.85154420029064E-16));
#7136=DIRECTION('ref_axis',(-1.85154420029064E-16,0.,1.));
#7137=DIRECTION('center_axis',(1.,1.4811191380744E-16,1.85154420029064E-16));
#7138=DIRECTION('ref_axis',(1.85154420029064E-16,0.,-1.));
#7139=DIRECTION('center_axis',(1.,1.4811191380744E-16,1.85154420029064E-16));
#7140=DIRECTION('ref_axis',(1.85154420029064E-16,0.,-1.));
#7141=DIRECTION('',(1.,1.4811191380744E-16,1.85154420029064E-16));
#7142=DIRECTION('',(1.,1.4811191380744E-16,1.85154420029064E-16));
#7143=DIRECTION('center_axis',(1.,1.4811191380744E-16,1.85154420029064E-16));
#7144=DIRECTION('ref_axis',(1.85154420029064E-16,0.,-1.));
#7145=DIRECTION('center_axis',(1.,1.4811191380744E-16,1.85154420029064E-16));
#7146=DIRECTION('ref_axis',(1.85154420029064E-16,0.,-1.));
#7147=DIRECTION('',(-1.,0.,-1.85037170770859E-16));
#7148=DIRECTION('center_axis',(1.,3.00568153244441E-16,7.87229747683671E-17));
#7149=DIRECTION('ref_axis',(-3.00568153244441E-16,1.,0.));
#7150=DIRECTION('',(-1.,0.,-1.96601993944038E-16));
#7151=DIRECTION('center_axis',(1.,3.00568153244441E-16,7.87229747683671E-17));
#7152=DIRECTION('ref_axis',(-3.00568153244441E-16,1.,0.));
#7153=DIRECTION('',(-1.,0.,0.));
#7154=DIRECTION('center_axis',(1.,4.06999598505139E-16,2.3117921420537E-16));
#7155=DIRECTION('ref_axis',(-4.06999598505139E-16,1.,0.));
#7156=DIRECTION('',(-1.,0.,0.));
#7157=DIRECTION('center_axis',(1.,4.06999598505139E-16,2.3117921420537E-16));
#7158=DIRECTION('ref_axis',(-4.06999598505139E-16,1.,0.));
#7159=DIRECTION('',(-1.,0.,-3.70074341541719E-16));
#7160=DIRECTION('center_axis',(1.,2.54543359068137E-16,3.37610659466067E-16));
#7161=DIRECTION('ref_axis',(3.37610659466067E-16,0.,-1.));
#7162=DIRECTION('',(-1.,0.,-3.70074341541719E-16));
#7163=DIRECTION('center_axis',(1.,2.54543359068137E-16,3.37610659466067E-16));
#7164=DIRECTION('ref_axis',(3.37610659466067E-16,0.,-1.));
#7165=DIRECTION('',(-1.,0.,-1.96601993944038E-16));
#7166=DIRECTION('center_axis',(1.,1.4811191380744E-16,1.85154420029064E-16));
#7167=DIRECTION('ref_axis',(1.85154420029064E-16,0.,-1.));
#7168=DIRECTION('',(-1.,0.,-1.38777878078144E-16));
#7169=DIRECTION('center_axis',(1.,1.4811191380744E-16,1.85154420029064E-16));
#7170=DIRECTION('ref_axis',(1.85154420029064E-16,0.,-1.));
#7171=DIRECTION('center_axis',(1.,1.4811191380744E-16,1.85154420029064E-16));
#7172=DIRECTION('ref_axis',(1.85154420029064E-16,0.,-1.));
#7173=DIRECTION('center_axis',(1.,1.4811191380744E-16,1.85154420029064E-16));
#7174=DIRECTION('ref_axis',(1.85154420029064E-16,0.,-1.));
#7175=DIRECTION('center_axis',(1.,1.4811191380744E-16,1.85154420029064E-16));
#7176=DIRECTION('ref_axis',(1.85154420029064E-16,0.,-1.));
#7177=DIRECTION('center_axis',(1.,1.4811191380744E-16,1.85154420029064E-16));
#7178=DIRECTION('ref_axis',(1.85154420029064E-16,0.,-1.));
#7179=DIRECTION('center_axis',(1.,1.4811191380744E-16,1.85154420029064E-16));
#7180=DIRECTION('ref_axis',(1.85154420029064E-16,0.,-1.));
#7181=DIRECTION('center_axis',(-1.,-1.4811191380744E-16,-1.85154420029064E-16));
#7182=DIRECTION('ref_axis',(-1.85154420029064E-16,0.,1.));
#7183=DIRECTION('center_axis',(1.,1.4811191380744E-16,1.85154420029064E-16));
#7184=DIRECTION('ref_axis',(1.85154420029064E-16,0.,-1.));
#7185=DIRECTION('',(-1.,0.,-1.92827419455378E-16));
#7186=DIRECTION('center_axis',(1.,1.4811191380744E-16,1.85154420029064E-16));
#7187=DIRECTION('ref_axis',(1.85154420029064E-16,0.,-1.));
#7188=DIRECTION('',(-1.,0.,-1.65280645247467E-16));
#7189=DIRECTION('center_axis',(1.,1.4811191380744E-16,1.85154420029064E-16));
#7190=DIRECTION('ref_axis',(1.85154420029064E-16,0.,-1.));
#7191=DIRECTION('center_axis',(1.,1.4811191380744E-16,1.85154420029064E-16));
#7192=DIRECTION('ref_axis',(1.85154420029064E-16,0.,-1.));
#7193=DIRECTION('center_axis',(1.,1.4811191380744E-16,1.85154420029064E-16));
#7194=DIRECTION('ref_axis',(1.85154420029064E-16,0.,-1.));
#7195=DIRECTION('center_axis',(1.,1.4811191380744E-16,1.85154420029064E-16));
#7196=DIRECTION('ref_axis',(1.85154420029064E-16,0.,-1.));
#7197=DIRECTION('center_axis',(1.,1.4811191380744E-16,1.85154420029064E-16));
#7198=DIRECTION('ref_axis',(1.85154420029064E-16,0.,-1.));
#7199=DIRECTION('center_axis',(1.,1.4811191380744E-16,1.85154420029064E-16));
#7200=DIRECTION('ref_axis',(3.15796771448933E-16,0.,-1.));
#7201=DIRECTION('center_axis',(1.,1.4811191380744E-16,1.85154420029064E-16));
#7202=DIRECTION('ref_axis',(3.15796771448933E-16,0.,-1.));
#7203=DIRECTION('center_axis',(1.,1.4811191380744E-16,1.85154420029064E-16));
#7204=DIRECTION('ref_axis',(1.85154420029064E-16,0.,-1.));
#7205=DIRECTION('center_axis',(-1.,-3.00568153244441E-16,-7.87229747683671E-17));
#7206=DIRECTION('ref_axis',(3.00568153244441E-16,-1.,0.));
#7207=DIRECTION('center_axis',(1.,3.00568153244441E-16,7.87229747683671E-17));
#7208=DIRECTION('ref_axis',(-3.0056815324444E-16,1.,-1.04744440165294E-14));
#7209=DIRECTION('',(-1.,0.,-5.50935484158224E-17));
#7210=DIRECTION('center_axis',(1.,3.00568153244441E-16,7.87229747683671E-17));
#7211=DIRECTION('ref_axis',(-3.0056815324444E-16,1.,-1.04744440165294E-14));
#7212=DIRECTION('',(-1.,0.,-8.26403226237337E-17));
#7213=DIRECTION('center_axis',(1.,3.00568153244441E-16,7.87229747683671E-17));
#7214=DIRECTION('ref_axis',(7.87229747683671E-17,0.,-1.));
#7215=DIRECTION('center_axis',(1.,3.00568153244441E-16,7.87229747683671E-17));
#7216=DIRECTION('ref_axis',(-3.00568153244441E-16,1.,0.));
#7217=DIRECTION('center_axis',(1.,3.00568153244441E-16,7.87229747683671E-17));
#7218=DIRECTION('ref_axis',(7.87229747683671E-17,0.,-1.));
#7219=DIRECTION('center_axis',(1.,3.00568153244441E-16,7.87229747683671E-17));
#7220=DIRECTION('ref_axis',(-3.00568153244441E-16,1.,0.));
#7221=DIRECTION('center_axis',(-1.,-4.06999598505139E-16,-2.3117921420537E-16));
#7222=DIRECTION('ref_axis',(4.06999598505139E-16,-1.,0.));
#7223=DIRECTION('center_axis',(1.,4.06999598505139E-16,2.3117921420537E-16));
#7224=DIRECTION('ref_axis',(-2.3117921420537E-16,-1.27744465495421E-32,
1.));
#7225=DIRECTION('',(-1.,-4.4074838732658E-16,-4.4074838732658E-16));
#7226=DIRECTION('center_axis',(1.,4.06999598505139E-16,2.3117921420537E-16));
#7227=DIRECTION('ref_axis',(-2.3117921420537E-16,-1.27744465495421E-32,
1.));
#7228=DIRECTION('',(-1.,-8.81496774653158E-16,-4.40748387326579E-16));
#7229=DIRECTION('center_axis',(1.,4.06999598505139E-16,2.3117921420537E-16));
#7230=DIRECTION('ref_axis',(2.3117921420537E-16,0.,-1.));
#7231=DIRECTION('center_axis',(1.,4.06999598505139E-16,2.3117921420537E-16));
#7232=DIRECTION('ref_axis',(-4.06999598505139E-16,1.,0.));
#7233=DIRECTION('center_axis',(1.,4.06999598505139E-16,2.3117921420537E-16));
#7234=DIRECTION('ref_axis',(2.3117921420537E-16,0.,-1.));
#7235=DIRECTION('center_axis',(1.,4.06999598505139E-16,2.3117921420537E-16));
#7236=DIRECTION('ref_axis',(-4.06999598505139E-16,1.,0.));
#7237=DIRECTION('center_axis',(-1.,-2.54543359068137E-16,-3.37610659466067E-16));
#7238=DIRECTION('ref_axis',(5.87374514062376E-17,0.707106781186545,-0.70710678118655));
#7239=DIRECTION('center_axis',(1.,2.54543359068137E-16,3.37610659466067E-16));
#7240=DIRECTION('ref_axis',(2.54543359068136E-16,-1.,3.49148133884313E-15));
#7241=DIRECTION('',(-1.,0.,0.));
#7242=DIRECTION('center_axis',(1.,2.54543359068137E-16,3.37610659466067E-16));
#7243=DIRECTION('ref_axis',(2.54543359068136E-16,-1.,3.49148133884313E-15));
#7244=DIRECTION('',(-1.,0.,-4.40748387326579E-16));
#7245=DIRECTION('center_axis',(1.,2.54543359068137E-16,3.37610659466067E-16));
#7246=DIRECTION('ref_axis',(3.37610659466067E-16,0.,-1.));
#7247=DIRECTION('center_axis',(1.,2.54543359068137E-16,3.37610659466067E-16));
#7248=DIRECTION('ref_axis',(3.37610659466067E-16,0.,-1.));
#7249=DIRECTION('center_axis',(1.,2.54543359068137E-16,3.37610659466067E-16));
#7250=DIRECTION('ref_axis',(3.37610659466067E-16,0.,-1.));
#7251=DIRECTION('center_axis',(1.,2.54543359068137E-16,3.37610659466067E-16));
#7252=DIRECTION('ref_axis',(3.37610659466067E-16,0.,-1.));
#7253=DIRECTION('center_axis',(1.,1.4811191380744E-16,1.85154420029064E-16));
#7254=DIRECTION('ref_axis',(1.85154420029064E-16,0.,-1.));
#7255=DIRECTION('center_axis',(1.,2.54543359068137E-16,3.37610659466067E-16));
#7256=DIRECTION('ref_axis',(3.15796771448933E-16,0.,-1.));
#7257=DIRECTION('center_axis',(1.,2.54543359068137E-16,3.37610659466067E-16));
#7258=DIRECTION('ref_axis',(3.15796771448933E-16,0.,-1.));
#7259=DIRECTION('center_axis',(1.,2.54543359068137E-16,3.37610659466067E-16));
#7260=DIRECTION('ref_axis',(-3.22551558256129E-16,-0.0570045103629633,0.99837392083241));
#7261=DIRECTION('center_axis',(1.,1.4811191380744E-16,1.85154420029064E-16));
#7262=DIRECTION('ref_axis',(-1.93296391409384E-16,0.0570045103629774,0.998373920832409));
#7263=DIRECTION('center_axis',(1.,4.06999598505139E-16,2.3117921420537E-16));
#7264=DIRECTION('ref_axis',(3.15796771448933E-16,0.,-1.));
#7265=DIRECTION('center_axis',(1.,4.06999598505139E-16,2.3117921420537E-16));
#7266=DIRECTION('ref_axis',(3.15796771448933E-16,0.,-1.));
#7267=DIRECTION('center_axis',(1.,4.06999598505139E-16,2.3117921420537E-16));
#7268=DIRECTION('ref_axis',(-4.06999598505139E-16,1.,0.));
#7269=DIRECTION('center_axis',(1.,1.4811191380744E-16,1.85154420029064E-16));
#7270=DIRECTION('ref_axis',(1.85154420029064E-16,0.,-1.));
#7271=DIRECTION('center_axis',(1.,3.00568153244441E-16,7.87229747683671E-17));
#7272=DIRECTION('ref_axis',(0.,0.,-1.));
#7273=DIRECTION('center_axis',(1.,3.00568153244441E-16,7.87229747683671E-17));
#7274=DIRECTION('ref_axis',(0.,0.,-1.));
#7275=DIRECTION('center_axis',(1.,3.00568153244441E-16,7.87229747683671E-17));
#7276=DIRECTION('ref_axis',(-3.00568153244441E-16,1.,0.));
#7277=DIRECTION('center_axis',(1.,1.4811191380744E-16,1.85154420029064E-16));
#7278=DIRECTION('ref_axis',(3.46606212565903E-16,0.,-1.));
#7279=DIRECTION('center_axis',(1.4811191380744E-16,-1.,3.20853184254275E-32));
#7280=DIRECTION('ref_axis',(-2.16628882853689E-16,0.,1.));
#7281=DIRECTION('center_axis',(1.,1.4811191380744E-16,1.85154420029064E-16));
#7282=DIRECTION('ref_axis',(3.46606212565902E-16,0.,-1.));
#7283=DIRECTION('center_axis',(1.4811191380744E-16,-1.,0.));
#7284=DIRECTION('ref_axis',(0.,0.,1.));
#7285=DIRECTION('center_axis',(1.,1.4811191380744E-16,1.85154420029064E-16));
#7286=DIRECTION('ref_axis',(1.85154420029064E-16,0.,-1.));
#7287=DIRECTION('',(1.,1.4811191380744E-16,1.85154420029064E-16));
#7288=DIRECTION('center_axis',(-1.,-1.4811191380744E-16,-1.85154420029064E-16));
#7289=DIRECTION('ref_axis',(-1.85154420029064E-16,0.,1.));
#7290=DIRECTION('center_axis',(-1.,-1.4811191380744E-16,-1.85154420029064E-16));
#7291=DIRECTION('ref_axis',(-1.85154420029064E-16,0.,1.));
#7292=DIRECTION('axis',(0.,0.,1.));
#7293=DIRECTION('refdir',(1.,0.,0.));
#7294=DIRECTION('center_axis',(-1.,-1.4811191380744E-16,-1.85154420029064E-16));
#7295=DIRECTION('ref_axis',(-1.85154420029064E-16,0.,1.));
#7296=DIRECTION('center_axis',(1.,1.4811191380744E-16,1.85154420029064E-16));
#7297=DIRECTION('ref_axis',(1.85154420029064E-16,0.,-1.));
#7298=DIRECTION('center_axis',(1.,1.4811191380744E-16,1.85154420029064E-16));
#7299=DIRECTION('ref_axis',(1.85154420029064E-16,0.,-1.));
#7300=DIRECTION('',(1.,1.4811191380744E-16,1.85154420029064E-16));
#7301=DIRECTION('',(1.,1.4811191380744E-16,1.85154420029064E-16));
#7302=DIRECTION('center_axis',(1.,1.4811191380744E-16,1.85154420029064E-16));
#7303=DIRECTION('ref_axis',(1.85154420029064E-16,0.,-1.));
#7304=DIRECTION('center_axis',(1.,1.4811191380744E-16,1.85154420029064E-16));
#7305=DIRECTION('ref_axis',(1.85154420029064E-16,0.,-1.));
#7306=DIRECTION('',(-1.,0.,-1.85037170770859E-16));
#7307=DIRECTION('center_axis',(1.,3.00568153244441E-16,7.87229747683671E-17));
#7308=DIRECTION('ref_axis',(-3.00568153244441E-16,1.,0.));
#7309=DIRECTION('',(-1.,0.,-1.96601993944038E-16));
#7310=DIRECTION('center_axis',(1.,3.00568153244441E-16,7.87229747683671E-17));
#7311=DIRECTION('ref_axis',(-3.00568153244441E-16,1.,0.));
#7312=DIRECTION('',(-1.,0.,0.));
#7313=DIRECTION('center_axis',(1.,4.06999598505139E-16,2.3117921420537E-16));
#7314=DIRECTION('ref_axis',(-4.06999598505139E-16,1.,0.));
#7315=DIRECTION('',(-1.,0.,0.));
#7316=DIRECTION('center_axis',(1.,4.06999598505139E-16,2.3117921420537E-16));
#7317=DIRECTION('ref_axis',(-4.06999598505139E-16,1.,0.));
#7318=DIRECTION('',(-1.,0.,-3.70074341541719E-16));
#7319=DIRECTION('center_axis',(1.,2.54543359068137E-16,3.37610659466067E-16));
#7320=DIRECTION('ref_axis',(3.37610659466067E-16,0.,-1.));
#7321=DIRECTION('',(-1.,0.,-3.70074341541719E-16));
#7322=DIRECTION('center_axis',(1.,2.54543359068137E-16,3.37610659466067E-16));
#7323=DIRECTION('ref_axis',(3.37610659466067E-16,0.,-1.));
#7324=DIRECTION('',(-1.,0.,-1.96601993944038E-16));
#7325=DIRECTION('center_axis',(1.,1.4811191380744E-16,1.85154420029064E-16));
#7326=DIRECTION('ref_axis',(1.85154420029064E-16,0.,-1.));
#7327=DIRECTION('',(-1.,0.,-1.38777878078144E-16));
#7328=DIRECTION('center_axis',(1.,1.4811191380744E-16,1.85154420029064E-16));
#7329=DIRECTION('ref_axis',(1.85154420029064E-16,0.,-1.));
#7330=DIRECTION('center_axis',(1.,1.4811191380744E-16,1.85154420029064E-16));
#7331=DIRECTION('ref_axis',(1.85154420029064E-16,0.,-1.));
#7332=DIRECTION('center_axis',(1.,1.4811191380744E-16,1.85154420029064E-16));
#7333=DIRECTION('ref_axis',(1.85154420029064E-16,0.,-1.));
#7334=DIRECTION('center_axis',(1.,1.4811191380744E-16,1.85154420029064E-16));
#7335=DIRECTION('ref_axis',(1.85154420029064E-16,0.,-1.));
#7336=DIRECTION('center_axis',(1.,1.4811191380744E-16,1.85154420029064E-16));
#7337=DIRECTION('ref_axis',(1.85154420029064E-16,0.,-1.));
#7338=DIRECTION('center_axis',(1.,1.4811191380744E-16,1.85154420029064E-16));
#7339=DIRECTION('ref_axis',(1.85154420029064E-16,0.,-1.));
#7340=DIRECTION('center_axis',(1.,1.4811191380744E-16,1.85154420029064E-16));
#7341=DIRECTION('ref_axis',(1.85154420029064E-16,0.,-1.));
#7342=DIRECTION('center_axis',(-1.,-1.4811191380744E-16,-1.85154420029064E-16));
#7343=DIRECTION('ref_axis',(-1.85154420029064E-16,0.,1.));
#7344=DIRECTION('center_axis',(1.,1.4811191380744E-16,1.85154420029064E-16));
#7345=DIRECTION('ref_axis',(1.85154420029064E-16,0.,-1.));
#7346=DIRECTION('',(-1.,0.,-1.92827419455378E-16));
#7347=DIRECTION('center_axis',(1.,1.4811191380744E-16,1.85154420029064E-16));
#7348=DIRECTION('ref_axis',(1.85154420029064E-16,0.,-1.));
#7349=DIRECTION('',(-1.,0.,-1.65280645247467E-16));
#7350=DIRECTION('center_axis',(1.,1.4811191380744E-16,1.85154420029064E-16));
#7351=DIRECTION('ref_axis',(1.85154420029064E-16,0.,-1.));
#7352=DIRECTION('center_axis',(1.,1.4811191380744E-16,1.85154420029064E-16));
#7353=DIRECTION('ref_axis',(1.85154420029064E-16,0.,-1.));
#7354=DIRECTION('center_axis',(1.,1.4811191380744E-16,1.85154420029064E-16));
#7355=DIRECTION('ref_axis',(1.85154420029064E-16,0.,-1.));
#7356=DIRECTION('center_axis',(1.,1.4811191380744E-16,1.85154420029064E-16));
#7357=DIRECTION('ref_axis',(1.85154420029064E-16,0.,-1.));
#7358=DIRECTION('center_axis',(1.,1.4811191380744E-16,1.85154420029064E-16));
#7359=DIRECTION('ref_axis',(1.85154420029064E-16,0.,-1.));
#7360=DIRECTION('center_axis',(1.,1.4811191380744E-16,1.85154420029064E-16));
#7361=DIRECTION('ref_axis',(3.15796771448933E-16,0.,-1.));
#7362=DIRECTION('center_axis',(1.,1.4811191380744E-16,1.85154420029064E-16));
#7363=DIRECTION('ref_axis',(3.15796771448933E-16,0.,-1.));
#7364=DIRECTION('center_axis',(1.,1.4811191380744E-16,1.85154420029064E-16));
#7365=DIRECTION('ref_axis',(1.85154420029064E-16,0.,-1.));
#7366=DIRECTION('center_axis',(-1.,-3.00568153244441E-16,-7.87229747683671E-17));
#7367=DIRECTION('ref_axis',(3.00568153244441E-16,-1.,0.));
#7368=DIRECTION('center_axis',(1.,3.00568153244441E-16,7.87229747683671E-17));
#7369=DIRECTION('ref_axis',(-3.0056815324444E-16,1.,-1.04744440165294E-14));
#7370=DIRECTION('',(-1.,0.,-5.50935484158224E-17));
#7371=DIRECTION('center_axis',(1.,3.00568153244441E-16,7.87229747683671E-17));
#7372=DIRECTION('ref_axis',(-3.0056815324444E-16,1.,-1.04744440165294E-14));
#7373=DIRECTION('',(-1.,0.,-8.26403226237337E-17));
#7374=DIRECTION('center_axis',(1.,3.00568153244441E-16,7.87229747683671E-17));
#7375=DIRECTION('ref_axis',(7.87229747683671E-17,0.,-1.));
#7376=DIRECTION('center_axis',(1.,3.00568153244441E-16,7.87229747683671E-17));
#7377=DIRECTION('ref_axis',(-3.00568153244441E-16,1.,0.));
#7378=DIRECTION('center_axis',(1.,3.00568153244441E-16,7.87229747683671E-17));
#7379=DIRECTION('ref_axis',(7.87229747683671E-17,0.,-1.));
#7380=DIRECTION('center_axis',(1.,3.00568153244441E-16,7.87229747683671E-17));
#7381=DIRECTION('ref_axis',(-3.00568153244441E-16,1.,0.));
#7382=DIRECTION('center_axis',(-1.,-4.06999598505139E-16,-2.3117921420537E-16));
#7383=DIRECTION('ref_axis',(4.06999598505139E-16,-1.,0.));
#7384=DIRECTION('center_axis',(1.,4.06999598505139E-16,2.3117921420537E-16));
#7385=DIRECTION('ref_axis',(-2.3117921420537E-16,-1.27744465495421E-32,
1.));
#7386=DIRECTION('',(-1.,-4.4074838732658E-16,-4.4074838732658E-16));
#7387=DIRECTION('center_axis',(1.,4.06999598505139E-16,2.3117921420537E-16));
#7388=DIRECTION('ref_axis',(-2.3117921420537E-16,-1.27744465495421E-32,
1.));
#7389=DIRECTION('',(-1.,-8.81496774653158E-16,-4.40748387326579E-16));
#7390=DIRECTION('center_axis',(1.,4.06999598505139E-16,2.3117921420537E-16));
#7391=DIRECTION('ref_axis',(2.3117921420537E-16,0.,-1.));
#7392=DIRECTION('center_axis',(1.,4.06999598505139E-16,2.3117921420537E-16));
#7393=DIRECTION('ref_axis',(-4.06999598505139E-16,1.,0.));
#7394=DIRECTION('center_axis',(1.,4.06999598505139E-16,2.3117921420537E-16));
#7395=DIRECTION('ref_axis',(2.3117921420537E-16,0.,-1.));
#7396=DIRECTION('center_axis',(1.,4.06999598505139E-16,2.3117921420537E-16));
#7397=DIRECTION('ref_axis',(-4.06999598505139E-16,1.,0.));
#7398=DIRECTION('center_axis',(-1.,-2.54543359068137E-16,-3.37610659466067E-16));
#7399=DIRECTION('ref_axis',(5.87374514062376E-17,0.707106781186545,-0.70710678118655));
#7400=DIRECTION('center_axis',(1.,2.54543359068137E-16,3.37610659466067E-16));
#7401=DIRECTION('ref_axis',(2.54543359068136E-16,-1.,3.49148133884313E-15));
#7402=DIRECTION('',(-1.,0.,0.));
#7403=DIRECTION('center_axis',(1.,2.54543359068137E-16,3.37610659466067E-16));
#7404=DIRECTION('ref_axis',(2.54543359068136E-16,-1.,3.49148133884313E-15));
#7405=DIRECTION('',(-1.,0.,-4.40748387326579E-16));
#7406=DIRECTION('center_axis',(1.,2.54543359068137E-16,3.37610659466067E-16));
#7407=DIRECTION('ref_axis',(3.37610659466067E-16,0.,-1.));
#7408=DIRECTION('center_axis',(1.,2.54543359068137E-16,3.37610659466067E-16));
#7409=DIRECTION('ref_axis',(3.37610659466067E-16,0.,-1.));
#7410=DIRECTION('center_axis',(1.,2.54543359068137E-16,3.37610659466067E-16));
#7411=DIRECTION('ref_axis',(3.37610659466067E-16,0.,-1.));
#7412=DIRECTION('center_axis',(1.,2.54543359068137E-16,3.37610659466067E-16));
#7413=DIRECTION('ref_axis',(3.37610659466067E-16,0.,-1.));
#7414=DIRECTION('center_axis',(1.,1.4811191380744E-16,1.85154420029064E-16));
#7415=DIRECTION('ref_axis',(1.85154420029064E-16,0.,-1.));
#7416=DIRECTION('center_axis',(1.,2.54543359068137E-16,3.37610659466067E-16));
#7417=DIRECTION('ref_axis',(3.15796771448933E-16,0.,-1.));
#7418=DIRECTION('center_axis',(1.,2.54543359068137E-16,3.37610659466067E-16));
#7419=DIRECTION('ref_axis',(3.15796771448933E-16,0.,-1.));
#7420=DIRECTION('center_axis',(1.,2.54543359068137E-16,3.37610659466067E-16));
#7421=DIRECTION('ref_axis',(-3.22551558256129E-16,-0.0570045103629633,0.99837392083241));
#7422=DIRECTION('center_axis',(1.,1.4811191380744E-16,1.85154420029064E-16));
#7423=DIRECTION('ref_axis',(-1.93296391409384E-16,0.0570045103629774,0.998373920832409));
#7424=DIRECTION('center_axis',(1.,4.06999598505139E-16,2.3117921420537E-16));
#7425=DIRECTION('ref_axis',(3.15796771448933E-16,0.,-1.));
#7426=DIRECTION('center_axis',(1.,4.06999598505139E-16,2.3117921420537E-16));
#7427=DIRECTION('ref_axis',(3.15796771448933E-16,0.,-1.));
#7428=DIRECTION('center_axis',(1.,4.06999598505139E-16,2.3117921420537E-16));
#7429=DIRECTION('ref_axis',(-4.06999598505139E-16,1.,0.));
#7430=DIRECTION('center_axis',(1.,1.4811191380744E-16,1.85154420029064E-16));
#7431=DIRECTION('ref_axis',(1.85154420029064E-16,0.,-1.));
#7432=DIRECTION('center_axis',(1.,3.00568153244441E-16,7.87229747683671E-17));
#7433=DIRECTION('ref_axis',(0.,0.,-1.));
#7434=DIRECTION('center_axis',(1.,3.00568153244441E-16,7.87229747683671E-17));
#7435=DIRECTION('ref_axis',(0.,0.,-1.));
#7436=DIRECTION('center_axis',(1.,3.00568153244441E-16,7.87229747683671E-17));
#7437=DIRECTION('ref_axis',(-3.00568153244441E-16,1.,0.));
#7438=DIRECTION('center_axis',(1.,1.4811191380744E-16,1.85154420029064E-16));
#7439=DIRECTION('ref_axis',(3.46606212565903E-16,0.,-1.));
#7440=DIRECTION('center_axis',(1.4811191380744E-16,-1.,3.20853184254275E-32));
#7441=DIRECTION('ref_axis',(-2.16628882853689E-16,0.,1.));
#7442=DIRECTION('center_axis',(1.,1.4811191380744E-16,1.85154420029064E-16));
#7443=DIRECTION('ref_axis',(3.46606212565902E-16,0.,-1.));
#7444=DIRECTION('center_axis',(1.4811191380744E-16,-1.,0.));
#7445=DIRECTION('ref_axis',(0.,0.,1.));
#7446=DIRECTION('center_axis',(1.,1.4811191380744E-16,1.85154420029064E-16));
#7447=DIRECTION('ref_axis',(1.85154420029064E-16,0.,-1.));
#7448=DIRECTION('',(1.,1.4811191380744E-16,1.85154420029064E-16));
#7449=DIRECTION('axis',(0.,0.,1.));
#7450=DIRECTION('refdir',(1.,0.,0.));
#7451=DIRECTION('axis',(0.,0.,1.));
#7452=DIRECTION('refdir',(1.,0.,0.));
#7453=DIRECTION('center_axis',(1.3988810110277E-14,0.,1.));
#7454=DIRECTION('ref_axis',(1.,0.,-1.3988810110277E-14));
#7455=DIRECTION('center_axis',(1.3988810110277E-14,0.,1.));
#7456=DIRECTION('ref_axis',(1.,0.,-1.3988810110277E-14));
#7457=DIRECTION('',(-0.86602540378444,-0.499999999999998,8.88178419698879E-15));
#7458=DIRECTION('center_axis',(-1.3988810110277E-14,0.,-1.));
#7459=DIRECTION('ref_axis',(1.,0.,-1.3988810110277E-14));
#7460=DIRECTION('',(-0.866025403784435,-0.500000000000007,1.77635683939776E-14));
#7461=DIRECTION('center_axis',(-0.499999999999999,0.866025403784439,6.99440505513849E-15));
#7462=DIRECTION('ref_axis',(0.,-8.07644328281097E-15,1.));
#7463=DIRECTION('',(0.866025403784439,0.499999999999999,0.));
#7464=DIRECTION('',(1.39967402747386E-14,0.,1.));
#7465=DIRECTION('',(1.39967402747386E-14,0.,1.));
#7466=DIRECTION('center_axis',(1.3988810110277E-14,0.,1.));
#7467=DIRECTION('ref_axis',(1.,0.,-1.3988810110277E-14));
#7468=DIRECTION('center_axis',(0.,0.,1.));
#7469=DIRECTION('ref_axis',(1.,0.,0.));
#7470=DIRECTION('',(1.39967402747385E-14,0.,1.));
#7471=DIRECTION('center_axis',(-0.500000000000006,0.866025403784435,6.96664947952286E-15));
#7472=DIRECTION('ref_axis',(1.39332989590456E-14,0.,1.));
#7473=DIRECTION('',(0.866025403784434,0.500000000000008,0.));
#7474=DIRECTION('',(1.39967402747385E-14,0.,1.));
#7475=DIRECTION('center_axis',(1.3988810110277E-14,0.,1.));
#7476=DIRECTION('ref_axis',(1.,0.,-1.3988810110277E-14));
#7477=DIRECTION('center_axis',(0.,0.,1.));
#7478=DIRECTION('ref_axis',(1.,0.,0.));
#7479=DIRECTION('center_axis',(0.,0.,1.));
#7480=DIRECTION('ref_axis',(1.,0.,0.));
#7481=DIRECTION('center_axis',(-0.866025403784443,0.,-0.499999999999992));
#7482=DIRECTION('ref_axis',(-0.499999999999992,0.,0.866025403784443));
#7483=DIRECTION('center_axis',(-0.866025403784443,0.,-0.499999999999992));
#7484=DIRECTION('ref_axis',(-0.499999999999992,0.,0.866025403784443));
#7485=DIRECTION('',(0.433012701892206,-0.5,-0.750000000000008));
#7486=DIRECTION('center_axis',(0.866025403784443,0.,0.499999999999992));
#7487=DIRECTION('ref_axis',(-0.499999999999992,0.,0.866025403784443));
#7488=DIRECTION('',(0.433012701892208,-0.500000000000003,-0.750000000000004));
#7489=DIRECTION('center_axis',(0.249999999999996,0.866025403784439,-0.433012701892221));
#7490=DIRECTION('ref_axis',(0.,0.447213595499959,0.894427190999915));
#7491=DIRECTION('',(-0.433012701892213,0.499999999999998,0.750000000000005));
#7492=DIRECTION('',(-0.866025403784443,0.,-0.499999999999992));
#7493=DIRECTION('',(-0.866025403784443,0.,-0.499999999999992));
#7494=DIRECTION('center_axis',(-0.866025403784443,0.,-0.499999999999992));
#7495=DIRECTION('ref_axis',(-0.499999999999992,0.,0.866025403784443));
#7496=DIRECTION('center_axis',(-0.866025403784443,0.,-0.499999999999992));
#7497=DIRECTION('ref_axis',(-0.499999999999992,0.,0.866025403784443));
#7498=DIRECTION('',(-0.866025403784443,0.,-0.499999999999992));
#7499=DIRECTION('center_axis',(0.249999999999999,0.866025403784435,-0.433012701892227));
#7500=DIRECTION('ref_axis',(-0.866025403784443,0.,-0.499999999999992));
#7501=DIRECTION('',(-0.433012701892207,0.50000000000001,0.750000000000001));
#7502=DIRECTION('',(-0.866025403784443,0.,-0.499999999999992));
#7503=DIRECTION('center_axis',(-0.866025403784443,0.,-0.499999999999992));
#7504=DIRECTION('ref_axis',(-0.499999999999992,0.,0.866025403784443));
#7505=DIRECTION('center_axis',(-0.866025403784443,0.,-0.499999999999992));
#7506=DIRECTION('ref_axis',(-0.499999999999992,0.,0.866025403784443));
#7507=DIRECTION('center_axis',(-0.866025403784443,0.,-0.499999999999992));
#7508=DIRECTION('ref_axis',(-0.499999999999992,0.,0.866025403784443));
#7509=DIRECTION('center_axis',(0.866025403784429,0.,-0.500000000000016));
#7510=DIRECTION('ref_axis',(-0.500000000000016,0.,-0.866025403784429));
#7511=DIRECTION('center_axis',(0.866025403784429,0.,-0.500000000000016));
#7512=DIRECTION('ref_axis',(-0.500000000000016,0.,-0.866025403784429));
#7513=DIRECTION('',(0.433012701892233,-0.5,0.749999999999992));
#7514=DIRECTION('center_axis',(-0.866025403784429,0.,0.500000000000016));
#7515=DIRECTION('ref_axis',(-0.500000000000016,0.,-0.866025403784429));
#7516=DIRECTION('',(0.433012701892229,-0.500000000000006,0.749999999999991));
#7517=DIRECTION('center_axis',(0.250000000000008,0.866025403784439,0.433012701892214));
#7518=DIRECTION('ref_axis',(0.,-0.447213595499953,0.894427190999918));
#7519=DIRECTION('',(-0.433012701892223,0.500000000000001,-0.749999999999997));
#7520=DIRECTION('',(0.866025403784429,0.,-0.500000000000016));
#7521=DIRECTION('',(0.866025403784429,0.,-0.500000000000016));
#7522=DIRECTION('center_axis',(0.866025403784429,0.,-0.500000000000016));
#7523=DIRECTION('ref_axis',(-0.500000000000016,0.,-0.866025403784429));
#7524=DIRECTION('center_axis',(0.866025403784436,0.,-0.500000000000004));
#7525=DIRECTION('ref_axis',(-0.500000000000004,0.,-0.866025403784436));
#7526=DIRECTION('',(0.866025403784429,0.,-0.500000000000016));
#7527=DIRECTION('center_axis',(0.250000000000011,0.866025403784435,0.43301270189222));
#7528=DIRECTION('ref_axis',(0.866025403784429,0.,-0.500000000000016));
#7529=DIRECTION('',(-0.433012701892228,0.500000000000006,-0.749999999999991));
#7530=DIRECTION('',(0.866025403784429,0.,-0.500000000000016));
#7531=DIRECTION('center_axis',(0.866025403784429,0.,-0.500000000000016));
#7532=DIRECTION('ref_axis',(-0.500000000000016,0.,-0.866025403784429));
#7533=DIRECTION('center_axis',(0.866025403784436,0.,-0.500000000000004));
#7534=DIRECTION('ref_axis',(-0.500000000000004,0.,-0.866025403784436));
#7535=DIRECTION('center_axis',(0.866025403784436,0.,-0.500000000000004));
#7536=DIRECTION('ref_axis',(-0.500000000000004,0.,-0.866025403784436));
#7537=DIRECTION('center_axis',(0.866025403784443,0.,0.499999999999992));
#7538=DIRECTION('ref_axis',(-0.321393804843261,0.766044443118984,0.556670399226416));
#7539=DIRECTION('',(0.866025403784442,0.,0.499999999999994));
#7540=DIRECTION('center_axis',(-0.866025403784443,0.,-0.499999999999992));
#7541=DIRECTION('ref_axis',(-0.499999999999992,0.,0.866025403784443));
#7542=DIRECTION('',(0.866025403784443,0.,0.499999999999992));
#7543=DIRECTION('center_axis',(-0.866025403784443,0.,-0.499999999999992));
#7544=DIRECTION('ref_axis',(-0.499999999999992,0.,0.866025403784443));
#7545=DIRECTION('center_axis',(0.866025403784443,0.,0.499999999999992));
#7546=DIRECTION('ref_axis',(0.499999999999992,0.,-0.866025403784443));
#7547=DIRECTION('',(0.866025403784443,0.,0.499999999999992));
#7548=DIRECTION('center_axis',(-0.866025403784443,0.,-0.499999999999992));
#7549=DIRECTION('ref_axis',(-0.499999999999992,0.,0.866025403784443));
#7550=DIRECTION('',(0.866025403784443,0.,0.499999999999992));
#7551=DIRECTION('center_axis',(-0.866025403784443,0.,-0.499999999999992));
#7552=DIRECTION('ref_axis',(-0.499999999999992,0.,0.866025403784443));
#7553=DIRECTION('center_axis',(0.866025403784443,0.,0.499999999999992));
#7554=DIRECTION('ref_axis',(0.499999999999992,0.,-0.866025403784443));
#7555=DIRECTION('',(0.866025403784443,0.,0.499999999999992));
#7556=DIRECTION('center_axis',(-0.866025403784443,0.,-0.499999999999992));
#7557=DIRECTION('ref_axis',(-0.499999999999992,0.,0.866025403784443));
#7558=DIRECTION('',(0.866025403784443,0.,0.499999999999993));
#7559=DIRECTION('center_axis',(-0.866025403784443,0.,-0.499999999999992));
#7560=DIRECTION('ref_axis',(-0.499999999999992,0.,0.866025403784443));
#7561=DIRECTION('center_axis',(-0.866025403784443,0.,-0.499999999999992));
#7562=DIRECTION('ref_axis',(-0.499999999999992,0.,0.866025403784443));
#7563=DIRECTION('',(-0.171010071662818,-0.939692620785907,0.296198132726037));
#7564=DIRECTION('',(-0.469846310392953,0.34202014332566,0.813797681349378));
#7565=DIRECTION('',(0.171010071662822,0.93969262078591,-0.296198132726026));
#7566=DIRECTION('',(-0.321393804843259,0.766044443118992,0.556670399226406));
#7567=DIRECTION('',(0.383022221559474,0.642787609686542,-0.663413948168944));
#7568=DIRECTION('',(0.32139380484327,-0.766044443118983,-0.556670399226412));
#7569=DIRECTION('',(0.492403876506091,0.173648177666908,-0.852868531952455));
#7570=DIRECTION('',(0.0868240888334702,-0.984807753012207,-0.150383733180441));
#7571=DIRECTION('',(-0.492403876506098,-0.173648177666911,0.852868531952451));
#7572=DIRECTION('center_axis',(-0.866025403784443,0.,-0.499999999999992));
#7573=DIRECTION('ref_axis',(-0.499999999999992,0.,0.866025403784443));
#7574=DIRECTION('center_axis',(-0.866025403784436,0.,0.500000000000004));
#7575=DIRECTION('ref_axis',(-0.321393804843269,0.766044443118983,-0.556670399226412));
#7576=DIRECTION('',(-0.866025403784437,0.,0.500000000000003));
#7577=DIRECTION('center_axis',(0.866025403784436,0.,-0.500000000000004));
#7578=DIRECTION('ref_axis',(-0.500000000000004,0.,-0.866025403784436));
#7579=DIRECTION('',(-0.866025403784436,0.,0.500000000000004));
#7580=DIRECTION('center_axis',(0.866025403784436,0.,-0.500000000000004));
#7581=DIRECTION('ref_axis',(-0.500000000000004,0.,-0.866025403784436));
#7582=DIRECTION('center_axis',(-0.866025403784436,0.,0.500000000000004));
#7583=DIRECTION('ref_axis',(0.500000000000004,0.,0.866025403784436));
#7584=DIRECTION('',(-0.866025403784436,0.,0.500000000000005));
#7585=DIRECTION('center_axis',(0.866025403784436,0.,-0.500000000000004));
#7586=DIRECTION('ref_axis',(-0.500000000000004,0.,-0.866025403784436));
#7587=DIRECTION('',(-0.866025403784435,0.,0.500000000000006));
#7588=DIRECTION('center_axis',(0.866025403784436,0.,-0.500000000000004));
#7589=DIRECTION('ref_axis',(-0.500000000000004,0.,-0.866025403784436));
#7590=DIRECTION('center_axis',(-0.866025403784436,0.,0.500000000000004));
#7591=DIRECTION('ref_axis',(0.500000000000004,0.,0.866025403784436));
#7592=DIRECTION('',(-0.866025403784436,0.,0.500000000000004));
#7593=DIRECTION('center_axis',(0.866025403784436,0.,-0.500000000000004));
#7594=DIRECTION('ref_axis',(-0.500000000000004,0.,-0.866025403784436));
#7595=DIRECTION('',(-0.866025403784436,0.,0.500000000000005));
#7596=DIRECTION('center_axis',(0.866025403784436,0.,-0.500000000000004));
#7597=DIRECTION('ref_axis',(-0.500000000000004,0.,-0.866025403784436));
#7598=DIRECTION('center_axis',(0.866025403784436,0.,-0.500000000000004));
#7599=DIRECTION('ref_axis',(-0.500000000000004,0.,-0.866025403784436));
#7600=DIRECTION('',(-0.171010071662835,-0.939692620785907,-0.296198132726028));
#7601=DIRECTION('',(-0.469846310392953,0.34202014332566,-0.813797681349378));
#7602=DIRECTION('',(0.171010071662839,0.93969262078591,0.296198132726018));
#7603=DIRECTION('',(-0.321393804843267,0.766044443118985,-0.556670399226411));
#7604=DIRECTION('',(0.383022221559487,0.642787609686547,0.663413948168932));
#7605=DIRECTION('',(0.321393804843261,-0.766044443118982,0.556670399226419));
#7606=DIRECTION('',(0.492403876506108,0.173648177666911,0.852868531952445));
#7607=DIRECTION('',(0.0868240888334687,-0.984807753012208,0.150383733180434));
#7608=DIRECTION('',(-0.492403876506111,-0.173648177666932,-0.852868531952439));
#7609=DIRECTION('center_axis',(0.866025403784436,0.,-0.500000000000004));
#7610=DIRECTION('ref_axis',(-0.500000000000004,0.,-0.866025403784436));
#7611=DIRECTION('center_axis',(0.,0.,-1.));
#7612=DIRECTION('ref_axis',(-1.,0.,0.));
#7613=DIRECTION('',(0.,0.,-1.));
#7614=DIRECTION('center_axis',(0.,0.,1.));
#7615=DIRECTION('ref_axis',(1.,0.,0.));
#7616=DIRECTION('',(0.,0.,-1.));
#7617=DIRECTION('center_axis',(0.,0.,1.));
#7618=DIRECTION('ref_axis',(1.,0.,0.));
#7619=DIRECTION('center_axis',(0.,0.,-1.));
#7620=DIRECTION('ref_axis',(-1.,0.,0.));
#7621=DIRECTION('',(0.,0.,-1.));
#7622=DIRECTION('center_axis',(0.,0.,1.));
#7623=DIRECTION('ref_axis',(1.,0.,0.));
#7624=DIRECTION('',(0.,0.,-1.));
#7625=DIRECTION('center_axis',(0.,0.,1.));
#7626=DIRECTION('ref_axis',(1.,0.,0.));
#7627=DIRECTION('center_axis',(0.,0.,-1.));
#7628=DIRECTION('ref_axis',(0.642787609686533,0.766044443118984,0.));
#7629=DIRECTION('',(0.,0.,-1.));
#7630=DIRECTION('center_axis',(0.,0.,1.));
#7631=DIRECTION('ref_axis',(1.,0.,0.));
#7632=DIRECTION('',(0.,0.,-1.));
#7633=DIRECTION('center_axis',(0.,0.,1.));
#7634=DIRECTION('ref_axis',(1.,0.,0.));
#7635=DIRECTION('center_axis',(0.,0.,1.));
#7636=DIRECTION('ref_axis',(1.,0.,0.));
#7637=DIRECTION('',(0.642787609686527,0.766044443118988,0.));
#7638=DIRECTION('',(-0.766044443118964,0.642787609686556,0.));
#7639=DIRECTION('',(-0.642787609686546,-0.766044443118973,0.));
#7640=DIRECTION('',(-0.984807753012213,0.173648177666901,0.));
#7641=DIRECTION('',(-0.173648177666935,-0.984807753012207,0.));
#7642=DIRECTION('',(0.984807753012211,-0.173648177666915,0.));
#7643=DIRECTION('',(0.342020143325671,-0.939692620785908,0.));
#7644=DIRECTION('',(0.939692620785911,0.342020143325661,0.));
#7645=DIRECTION('',(-0.342020143325671,0.939692620785908,0.));
#7646=DIRECTION('center_axis',(0.,0.,1.));
#7647=DIRECTION('ref_axis',(1.,0.,0.));
#7648=DIRECTION('center_axis',(0.,-1.,0.));
#7649=DIRECTION('ref_axis',(0.,0.,-1.));
#7650=DIRECTION('center_axis',(0.,1.,0.));
#7651=DIRECTION('ref_axis',(0.,0.,1.));
#7652=DIRECTION('',(0.,1.,0.));
#7653=DIRECTION('',(0.,1.,0.));
#7654=DIRECTION('center_axis',(0.,1.,0.));
#7655=DIRECTION('ref_axis',(0.,0.,1.));
#7656=DIRECTION('center_axis',(0.,1.,0.));
#7657=DIRECTION('ref_axis',(0.,0.,1.));
#7658=DIRECTION('center_axis',(0.,1.,0.));
#7659=DIRECTION('ref_axis',(0.,0.,1.));
#7660=DIRECTION('center_axis',(0.,1.,0.));
#7661=DIRECTION('ref_axis',(0.,0.,1.));
#7662=DIRECTION('center_axis',(0.,-1.,0.));
#7663=DIRECTION('ref_axis',(0.,0.,-1.));
#7664=DIRECTION('center_axis',(0.,1.,0.));
#7665=DIRECTION('ref_axis',(0.,0.,1.));
#7666=DIRECTION('center_axis',(0.,1.,0.));
#7667=DIRECTION('ref_axis',(0.,0.,1.));
#7668=DIRECTION('',(0.,1.,0.));
#7669=DIRECTION('center_axis',(0.,1.,0.));
#7670=DIRECTION('ref_axis',(0.,0.,1.));
#7671=DIRECTION('center_axis',(0.,0.,1.));
#7672=DIRECTION('ref_axis',(1.,0.,0.));
#7673=DIRECTION('center_axis',(0.,0.,1.));
#7674=DIRECTION('ref_axis',(1.,0.,0.));
#7675=DIRECTION('',(0.,0.,-1.));
#7676=DIRECTION('center_axis',(0.,0.,1.));
#7677=DIRECTION('ref_axis',(1.,0.,0.));
#7678=DIRECTION('center_axis',(0.,0.,1.));
#7679=DIRECTION('ref_axis',(1.,0.,0.));
#7680=DIRECTION('',(-0.642787609686536,-0.766044443118981,0.));
#7681=DIRECTION('',(-0.76604444311897,0.642787609686548,0.));
#7682=DIRECTION('',(-0.642787609686528,-0.766044443118987,0.));
#7683=DIRECTION('',(-0.342020143325666,0.939692620785909,0.));
#7684=DIRECTION('',(0.939692620785913,0.342020143325658,0.));
#7685=DIRECTION('',(-0.342020143325671,0.939692620785908,0.));
#7686=DIRECTION('',(0.984807753012212,-0.173648177666909,0.));
#7687=DIRECTION('',(-0.173648177666936,-0.984807753012207,0.));
#7688=DIRECTION('',(0.98480775301221,-0.173648177666918,0.));
#7689=DIRECTION('center_axis',(0.,0.,-1.));
#7690=DIRECTION('ref_axis',(-1.,0.,0.));
#7691=DIRECTION('center_axis',(0.,0.,1.));
#7692=DIRECTION('ref_axis',(1.,0.,0.));
#7693=DIRECTION('center_axis',(0.,0.,1.));
#7694=DIRECTION('ref_axis',(1.,0.,0.));
#7695=DIRECTION('',(0.,0.,1.));
#7696=DIRECTION('center_axis',(0.,0.,1.));
#7697=DIRECTION('ref_axis',(1.,0.,0.));
#7698=DIRECTION('',(0.,0.,1.));
#7699=DIRECTION('center_axis',(0.,0.,1.));
#7700=DIRECTION('ref_axis',(1.,0.,0.));
#7701=DIRECTION('',(0.707106781186548,8.65956056235493E-17,-0.707106781186548));
#7702=DIRECTION('center_axis',(0.866025403784443,0.,-0.499999999999992));
#7703=DIRECTION('ref_axis',(-0.499999999999992,0.,-0.866025403784443));
#7704=DIRECTION('center_axis',(0.866025403784443,0.,-0.499999999999992));
#7705=DIRECTION('ref_axis',(-0.499999999999992,0.,-0.866025403784443));
#7706=DIRECTION('',(-0.866025403784443,0.,0.499999999999992));
#7707=DIRECTION('center_axis',(-0.866025403784436,0.,-0.500000000000004));
#7708=DIRECTION('ref_axis',(-0.500000000000004,0.,0.866025403784436));
#7709=DIRECTION('center_axis',(-0.866025403784436,0.,-0.500000000000004));
#7710=DIRECTION('ref_axis',(-0.500000000000004,0.,0.866025403784436));
#7711=DIRECTION('',(0.866025403784436,0.,0.500000000000004));
#7712=DIRECTION('center_axis',(-0.866025403784443,0.,-0.499999999999992));
#7713=DIRECTION('ref_axis',(-0.499999999999992,0.,0.866025403784443));
#7714=DIRECTION('center_axis',(-0.866025403784443,0.,-0.499999999999992));
#7715=DIRECTION('ref_axis',(-0.499999999999992,0.,0.866025403784443));
#7716=DIRECTION('',(0.171010071662833,0.939692620785909,-0.296198132726024));
#7717=DIRECTION('',(-0.492403876506096,-0.17364817766691,0.852868531952452));
#7718=DIRECTION('',(0.0868240888334701,-0.984807753012206,-0.150383733180445));
#7719=DIRECTION('',(-0.4924038765061,-0.173648177666906,0.85286853195245));
#7720=DIRECTION('',(0.321393804843263,-0.766044443118983,-0.556670399226417));
#7721=DIRECTION('',(0.383022221559485,0.642787609686548,-0.663413948168932));
#7722=DIRECTION('',(0.321393804843258,-0.766044443118986,-0.556670399226415));
#7723=DIRECTION('',(0.171010071662833,0.939692620785909,-0.296198132726024));
#7724=DIRECTION('',(-0.469846310392945,0.342020143325657,0.813797681349384));
#7725=DIRECTION('center_axis',(0.866025403784443,0.,0.499999999999992));
#7726=DIRECTION('ref_axis',(0.499999999999992,0.,-0.866025403784443));
#7727=DIRECTION('center_axis',(-0.866025403784445,0.,-0.49999999999999));
#7728=DIRECTION('ref_axis',(-0.49999999999999,0.,0.866025403784445));
#7729=DIRECTION('center_axis',(-0.866025403784445,0.,-0.49999999999999));
#7730=DIRECTION('ref_axis',(-0.49999999999999,0.,0.866025403784445));
#7731=DIRECTION('',(-0.866025403784443,0.,-0.499999999999992));
#7732=DIRECTION('center_axis',(0.866025403784436,0.,-0.500000000000004));
#7733=DIRECTION('ref_axis',(-0.500000000000004,0.,-0.866025403784436));
#7734=DIRECTION('center_axis',(0.866025403784436,0.,-0.500000000000004));
#7735=DIRECTION('ref_axis',(-0.500000000000004,0.,-0.866025403784436));
#7736=DIRECTION('',(0.171010071662833,0.939692620785909,0.296198132726024));
#7737=DIRECTION('',(-0.49240387650611,-0.173648177666926,-0.852868531952441));
#7738=DIRECTION('',(0.0868240888334687,-0.984807753012208,0.150383733180434));
#7739=DIRECTION('',(-0.492403876506114,-0.173648177666907,-0.852868531952442));
#7740=DIRECTION('',(0.321393804843267,-0.766044443118988,0.556670399226408));
#7741=DIRECTION('',(0.383022221559495,0.64278760968655,0.663413948168925));
#7742=DIRECTION('',(0.321393804843269,-0.766044443118987,0.556670399226408));
#7743=DIRECTION('',(0.171010071662833,0.939692620785909,0.296198132726024));
#7744=DIRECTION('',(-0.469846310392969,0.342020143325655,-0.813797681349371));
#7745=DIRECTION('center_axis',(-0.866025403784436,0.,0.500000000000004));
#7746=DIRECTION('ref_axis',(0.500000000000004,0.,0.866025403784436));
#7747=DIRECTION('center_axis',(0.866025403784436,0.,-0.500000000000004));
#7748=DIRECTION('ref_axis',(-0.500000000000004,0.,-0.866025403784436));
#7749=DIRECTION('center_axis',(0.866025403784436,0.,-0.500000000000004));
#7750=DIRECTION('ref_axis',(-0.500000000000004,0.,-0.866025403784436));
#7751=DIRECTION('',(0.866025403784436,0.,-0.500000000000004));
#7752=DIRECTION('center_axis',(-0.866025403784436,0.,-0.500000000000004));
#7753=DIRECTION('ref_axis',(-0.500000000000004,0.,0.866025403784436));
#7754=DIRECTION('',(-0.866025403784436,0.,-0.500000000000004));
#7755=DIRECTION('center_axis',(0.866025403784443,0.,-0.499999999999992));
#7756=DIRECTION('ref_axis',(-0.499999999999992,0.,-0.866025403784443));
#7757=DIRECTION('',(0.866025403784443,0.,-0.499999999999992));
#7758=DIRECTION('center_axis',(0.866025403784436,0.,-0.500000000000004));
#7759=DIRECTION('ref_axis',(-0.500000000000004,0.,-0.866025403784436));
#7760=DIRECTION('',(-0.965925826289069,8.65956056235496E-17,-0.258819045102519));
#7761=DIRECTION('center_axis',(-0.866025403784445,0.,-0.49999999999999));
#7762=DIRECTION('ref_axis',(-0.49999999999999,0.,0.866025403784445));
#7763=DIRECTION('',(0.258819045102533,8.65956056235492E-17,0.965925826289065));
#7764=DIRECTION('center_axis',(0.,1.,0.));
#7765=DIRECTION('ref_axis',(0.,0.,1.));
#7766=DIRECTION('center_axis',(0.,1.,0.));
#7767=DIRECTION('ref_axis',(0.,0.,1.));
#7768=DIRECTION('center_axis',(0.,-1.,0.));
#7769=DIRECTION('ref_axis',(0.,0.,-1.));
#7770=DIRECTION('',(0.,-1.,0.));
#7771=DIRECTION('',(0.,-1.,0.));
#7772=DIRECTION('center_axis',(-0.939692620785908,-0.342020143325669,0.));
#7773=DIRECTION('ref_axis',(0.,0.,1.));
#7774=DIRECTION('',(0.,0.,1.));
#7775=DIRECTION('center_axis',(0.939692620785908,0.342020143325669,0.));
#7776=DIRECTION('ref_axis',(0.,0.,-1.));
#7777=DIRECTION('',(0.,0.,-1.));
#7778=DIRECTION('center_axis',(0.342020143325655,-0.939692620785914,0.));
#7779=DIRECTION('ref_axis',(0.,0.,-1.));
#7780=DIRECTION('center_axis',(0.173648177666921,0.98480775301221,0.));
#7781=DIRECTION('ref_axis',(0.,0.,1.));
#7782=DIRECTION('',(0.,0.,1.));
#7783=DIRECTION('center_axis',(-0.173648177666921,-0.98480775301221,0.));
#7784=DIRECTION('ref_axis',(0.,0.,-1.));
#7785=DIRECTION('',(0.,0.,-1.));
#7786=DIRECTION('center_axis',(-0.984807753012207,0.173648177666936,0.));
#7787=DIRECTION('ref_axis',(0.,0.,1.));
#7788=DIRECTION('center_axis',(0.766044443118981,-0.642787609686535,0.));
#7789=DIRECTION('ref_axis',(0.,0.,-1.));
#7790=DIRECTION('',(0.,0.,1.));
#7791=DIRECTION('center_axis',(-0.766044443118981,0.642787609686535,0.));
#7792=DIRECTION('ref_axis',(0.,0.,1.));
#7793=DIRECTION('',(0.,0.,-1.));
#7794=DIRECTION('center_axis',(0.642787609686547,0.766044443118972,0.));
#7795=DIRECTION('ref_axis',(0.,0.,-1.));
#7796=DIRECTION('center_axis',(-0.0868240888334609,0.98480775301221,-0.150383733180426));
#7797=DIRECTION('ref_axis',(0.,0.150953786239872,0.98854082081614));
#7798=DIRECTION('',(0.866025403784436,0.,-0.500000000000005));
#7799=DIRECTION('center_axis',(0.0868240888334609,-0.98480775301221,0.150383733180426));
#7800=DIRECTION('ref_axis',(0.,-0.150953786239872,-0.98854082081614));
#7801=DIRECTION('',(-0.866025403784436,0.,0.500000000000005));
#7802=DIRECTION('center_axis',(0.492403876506108,0.173648177666936,0.85286853195244));
#7803=DIRECTION('ref_axis',(0.866025403784436,0.,-0.500000000000004));
#7804=DIRECTION('center_axis',(-0.383022221559494,-0.642787609686535,-0.66341394816894));
#7805=DIRECTION('ref_axis',(-0.866025403784436,0.,0.500000000000004));
#7806=DIRECTION('',(0.866025403784436,0.,-0.500000000000005));
#7807=DIRECTION('center_axis',(0.383022221559494,0.642787609686535,0.66341394816894));
#7808=DIRECTION('ref_axis',(0.866025403784436,0.,-0.500000000000004));
#7809=DIRECTION('',(-0.866025403784436,0.,0.500000000000005));
#7810=DIRECTION('center_axis',(-0.321393804843276,0.766044443118972,-0.556670399226425));
#7811=DIRECTION('ref_axis',(-0.866025403784436,0.,0.500000000000004));
#7812=DIRECTION('center_axis',(0.469846310392958,-0.342020143325669,0.813797681349371));
#7813=DIRECTION('ref_axis',(0.866025403784436,0.,-0.500000000000004));
#7814=DIRECTION('',(0.866025403784437,0.,-0.500000000000003));
#7815=DIRECTION('center_axis',(-0.469846310392958,0.342020143325669,-0.813797681349371));
#7816=DIRECTION('ref_axis',(-0.866025403784436,0.,0.500000000000004));
#7817=DIRECTION('',(-0.866025403784437,0.,0.500000000000003));
#7818=DIRECTION('center_axis',(-0.171010071662829,-0.939692620785914,-0.296198132726011));
#7819=DIRECTION('ref_axis',(0.,0.300626578483209,-0.953741925422952));
#7820=DIRECTION('center_axis',(-0.0868240888334589,0.98480775301221,0.150383733180428));
#7821=DIRECTION('ref_axis',(0.,-0.150953786239873,0.988540820816139));
#7822=DIRECTION('',(-0.866025403784443,0.,-0.499999999999992));
#7823=DIRECTION('center_axis',(0.0868240888334589,-0.98480775301221,-0.150383733180428));
#7824=DIRECTION('ref_axis',(0.,0.150953786239873,-0.988540820816139));
#7825=DIRECTION('',(0.866025403784443,0.,0.499999999999992));
#7826=DIRECTION('center_axis',(0.492403876506096,0.173648177666936,-0.852868531952447));
#7827=DIRECTION('ref_axis',(-0.866025403784443,0.,-0.499999999999992));
#7828=DIRECTION('center_axis',(-0.383022221559485,-0.642787609686535,0.663413948168945));
#7829=DIRECTION('ref_axis',(0.866025403784443,0.,0.499999999999992));
#7830=DIRECTION('',(-0.866025403784443,0.,-0.499999999999992));
#7831=DIRECTION('center_axis',(0.383022221559485,0.642787609686535,-0.663413948168945));
#7832=DIRECTION('ref_axis',(-0.866025403784443,0.,-0.499999999999992));
#7833=DIRECTION('',(0.866025403784443,0.,0.499999999999992));
#7834=DIRECTION('center_axis',(-0.321393804843268,0.766044443118972,0.556670399226429));
#7835=DIRECTION('ref_axis',(0.866025403784443,0.,0.499999999999992));
#7836=DIRECTION('center_axis',(0.469846310392947,-0.342020143325669,-0.813797681349378));
#7837=DIRECTION('ref_axis',(-0.866025403784443,0.,-0.499999999999992));
#7838=DIRECTION('',(-0.866025403784443,0.,-0.499999999999992));
#7839=DIRECTION('center_axis',(-0.469846310392947,0.342020143325669,0.813797681349378));
#7840=DIRECTION('ref_axis',(0.866025403784443,0.,0.499999999999992));
#7841=DIRECTION('',(0.866025403784443,0.,0.499999999999992));
#7842=DIRECTION('center_axis',(-0.171010071662825,-0.939692620785914,0.296198132726013));
#7843=DIRECTION('ref_axis',(0.,-0.300626578483211,-0.953741925422951));
#7844=DIRECTION('axis',(0.,0.,1.));
#7845=DIRECTION('refdir',(1.,0.,0.));
#7846=DIRECTION('center_axis',(-0.433012701892223,0.866025403784436,-0.250000000000002));
#7847=DIRECTION('ref_axis',(-0.894427190999914,-0.447213595499962,0.));
#7848=DIRECTION('center_axis',(0.433012701892223,-0.866025403784436,0.250000000000002));
#7849=DIRECTION('ref_axis',(0.894427190999914,0.447213595499962,0.));
#7850=DIRECTION('',(0.433012701892223,-0.866025403784436,0.250000000000002));
#7851=DIRECTION('center_axis',(0.433012701892223,-0.866025403784436,0.250000000000002));
#7852=DIRECTION('ref_axis',(0.894427190999914,0.447213595499962,0.));
#7853=DIRECTION('center_axis',(0.433012701892223,-0.866025403784436,0.250000000000002));
#7854=DIRECTION('ref_axis',(0.5,0.,-0.866025403784439));
#7855=DIRECTION('center_axis',(0.433012701892223,-0.866025403784437,0.250000000000002));
#7856=DIRECTION('ref_axis',(0.894427190999914,0.447213595499962,0.));
#7857=DIRECTION('center_axis',(0.433012701892223,-0.866025403784436,0.250000000000002));
#7858=DIRECTION('ref_axis',(0.5,0.,-0.866025403784439));
#7859=DIRECTION('center_axis',(-0.433012701892223,0.866025403784436,-0.250000000000002));
#7860=DIRECTION('ref_axis',(-0.894427190999914,-0.447213595499962,0.));
#7861=DIRECTION('center_axis',(-0.433012701892223,0.866025403784436,-0.250000000000002));
#7862=DIRECTION('ref_axis',(-0.894427190999914,-0.447213595499962,0.));
#7863=DIRECTION('center_axis',(0.433012701892223,-0.866025403784437,0.250000000000002));
#7864=DIRECTION('ref_axis',(0.894427190999914,0.447213595499962,0.));
#7865=DIRECTION('',(-0.433012701892223,0.866025403784436,-0.250000000000002));
#7866=DIRECTION('center_axis',(-0.433012701892223,0.866025403784436,-0.250000000000002));
#7867=DIRECTION('ref_axis',(-0.894427190999914,-0.447213595499962,0.));
#7868=DIRECTION('center_axis',(-0.433012701892223,0.866025403784436,-0.250000000000002));
#7869=DIRECTION('ref_axis',(-0.894427190999914,-0.447213595499962,0.));
#7870=DIRECTION('',(0.326269314185767,0.928600201712636,-0.17677669529664));
#7871=DIRECTION('center_axis',(0.433012701892223,-0.866025403784437,0.250000000000002));
#7872=DIRECTION('ref_axis',(0.5,0.,-0.866025403784439));
#7873=DIRECTION('center_axis',(0.433012701892223,-0.866025403784437,0.250000000000002));
#7874=DIRECTION('ref_axis',(0.894427190999914,0.447213595499962,0.));
#7875=DIRECTION('center_axis',(-0.433012701892223,0.866025403784436,-0.250000000000002));
#7876=DIRECTION('ref_axis',(-0.894427190999914,-0.447213595499962,0.));
#7877=DIRECTION('',(0.433012701892223,-0.866025403784436,0.250000000000002));
#7878=DIRECTION('axis',(0.,0.,1.));
#7879=DIRECTION('refdir',(1.,0.,0.));
#7880=DIRECTION('center_axis',(-0.612372435695796,0.707106781186546,-0.353553390593275));
#7881=DIRECTION('ref_axis',(-0.755928946018453,-0.654653670707979,0.));
#7882=DIRECTION('center_axis',(0.612372435695796,-0.707106781186546,0.353553390593275));
#7883=DIRECTION('ref_axis',(0.755928946018453,0.654653670707979,0.));
#7884=DIRECTION('',(0.612372435695796,-0.707106781186546,0.353553390593275));
#7885=DIRECTION('center_axis',(0.612372435695796,-0.707106781186546,0.353553390593275));
#7886=DIRECTION('ref_axis',(0.755928946018453,0.654653670707979,0.));
#7887=DIRECTION('center_axis',(0.612372435695796,-0.707106781186546,0.353553390593275));
#7888=DIRECTION('ref_axis',(0.5,0.,-0.866025403784438));
#7889=DIRECTION('center_axis',(0.612372435695796,-0.707106781186546,0.353553390593275));
#7890=DIRECTION('ref_axis',(0.755928946018453,0.654653670707979,0.));
#7891=DIRECTION('center_axis',(0.612372435695796,-0.707106781186546,0.353553390593275));
#7892=DIRECTION('ref_axis',(0.5,0.,-0.866025403784438));
#7893=DIRECTION('center_axis',(-0.612372435695796,0.707106781186546,-0.353553390593275));
#7894=DIRECTION('ref_axis',(-0.755928946018453,-0.654653670707979,0.));
#7895=DIRECTION('center_axis',(-0.612372435695796,0.707106781186546,-0.353553390593275));
#7896=DIRECTION('ref_axis',(-0.755928946018453,-0.654653670707979,0.));
#7897=DIRECTION('center_axis',(0.612372435695796,-0.707106781186546,0.353553390593275));
#7898=DIRECTION('ref_axis',(0.755928946018453,0.654653670707979,0.));
#7899=DIRECTION('',(-0.612372435695796,0.707106781186546,-0.353553390593275));
#7900=DIRECTION('center_axis',(-0.612372435695796,0.707106781186546,-0.353553390593275));
#7901=DIRECTION('ref_axis',(-0.755928946018453,-0.654653670707979,0.));
#7902=DIRECTION('center_axis',(-0.612372435695796,0.707106781186546,-0.353553390593275));
#7903=DIRECTION('ref_axis',(-0.755928946018453,-0.654653670707979,0.));
#7904=DIRECTION('',(0.101509781932626,0.962910049886276,-0.250000000000001));
#7905=DIRECTION('center_axis',(0.612372435695796,-0.707106781186546,0.353553390593275));
#7906=DIRECTION('ref_axis',(0.5,0.,-0.866025403784438));
#7907=DIRECTION('center_axis',(0.612372435695796,-0.707106781186546,0.353553390593275));
#7908=DIRECTION('ref_axis',(0.755928946018453,0.654653670707979,0.));
#7909=DIRECTION('center_axis',(-0.612372435695796,0.707106781186546,-0.353553390593275));
#7910=DIRECTION('ref_axis',(-0.755928946018453,-0.654653670707979,0.));
#7911=DIRECTION('',(0.612372435695796,-0.707106781186546,0.353553390593275));
#7912=DIRECTION('axis',(0.,0.,1.));
#7913=DIRECTION('refdir',(1.,0.,0.));
#7914=DIRECTION('center_axis',(-0.224143868042018,0.965925826289067,-0.129409522551263));
#7915=DIRECTION('ref_axis',(-0.974116947696296,-0.22604462437946,0.));
#7916=DIRECTION('center_axis',(0.224143868042018,-0.965925826289067,0.129409522551263));
#7917=DIRECTION('ref_axis',(0.974116947696296,0.22604462437946,0.));
#7918=DIRECTION('',(0.224143868042018,-0.965925826289067,0.129409522551263));
#7919=DIRECTION('center_axis',(0.224143868042018,-0.965925826289067,0.129409522551263));
#7920=DIRECTION('ref_axis',(0.974116947696296,0.22604462437946,0.));
#7921=DIRECTION('center_axis',(0.224143868042018,-0.965925826289067,0.129409522551263));
#7922=DIRECTION('ref_axis',(0.,-0.132788176096111,-0.991144439670156));
#7923=DIRECTION('center_axis',(0.224143868042018,-0.965925826289067,0.129409522551263));
#7924=DIRECTION('ref_axis',(0.974116947696296,0.22604462437946,0.));
#7925=DIRECTION('center_axis',(0.224143868042018,-0.965925826289067,0.129409522551263));
#7926=DIRECTION('ref_axis',(0.,-0.132788176096111,-0.991144439670156));
#7927=DIRECTION('center_axis',(-0.224143868042018,0.965925826289067,-0.129409522551263));
#7928=DIRECTION('ref_axis',(-0.974116947696296,-0.22604462437946,0.));
#7929=DIRECTION('center_axis',(-0.224143868042018,0.965925826289067,-0.129409522551263));
#7930=DIRECTION('ref_axis',(-0.974116947696296,-0.22604462437946,0.));
#7931=DIRECTION('center_axis',(0.224143868042018,-0.965925826289067,0.129409522551263));
#7932=DIRECTION('ref_axis',(0.974116947696296,0.22604462437946,0.));
#7933=DIRECTION('',(-0.224143868042018,0.965925826289067,-0.129409522551263));
#7934=DIRECTION('center_axis',(-0.224143868042018,0.965925826289067,-0.129409522551263));
#7935=DIRECTION('ref_axis',(-0.974116947696296,-0.22604462437946,0.));
#7936=DIRECTION('center_axis',(-0.224143868042018,0.965925826289067,-0.129409522551263));
#7937=DIRECTION('ref_axis',(-0.974116947696296,-0.22604462437946,0.));
#7938=DIRECTION('',(0.530311050330904,0.842850388641698,-0.091506350946111));
#7939=DIRECTION('center_axis',(0.224143868042018,-0.965925826289067,0.129409522551263));
#7940=DIRECTION('ref_axis',(0.,-0.132788176096111,-0.991144439670156));
#7941=DIRECTION('center_axis',(0.224143868042018,-0.965925826289067,0.129409522551263));
#7942=DIRECTION('ref_axis',(0.974116947696296,0.22604462437946,0.));
#7943=DIRECTION('center_axis',(-0.224143868042018,0.965925826289067,-0.129409522551263));
#7944=DIRECTION('ref_axis',(-0.974116947696296,-0.22604462437946,0.));
#7945=DIRECTION('',(0.224143868042018,-0.965925826289067,0.129409522551263));
#7946=DIRECTION('axis',(0.,0.,1.));
#7947=DIRECTION('refdir',(1.,0.,0.));
#7948=DIRECTION('center_axis',(0.,1.,0.));
#7949=DIRECTION('ref_axis',(0.,0.,1.));
#7950=DIRECTION('center_axis',(0.,1.,0.));
#7951=DIRECTION('ref_axis',(0.,0.,1.));
#7952=DIRECTION('',(0.,-1.,0.));
#7953=DIRECTION('center_axis',(0.,1.,0.));
#7954=DIRECTION('ref_axis',(0.,0.,1.));
#7955=DIRECTION('center_axis',(0.,1.,0.));
#7956=DIRECTION('ref_axis',(0.,0.,1.));
#7957=DIRECTION('center_axis',(0.,-1.,0.));
#7958=DIRECTION('ref_axis',(0.,0.,-1.));
#7959=DIRECTION('center_axis',(0.,1.,0.));
#7960=DIRECTION('ref_axis',(0.,0.,1.));
#7961=DIRECTION('center_axis',(0.,1.,0.));
#7962=DIRECTION('ref_axis',(0.,0.,1.));
#7963=DIRECTION('center_axis',(0.,1.,0.));
#7964=DIRECTION('ref_axis',(0.,0.,1.));
#7965=DIRECTION('center_axis',(0.,1.,0.));
#7966=DIRECTION('ref_axis',(0.,0.,1.));
#7967=DIRECTION('',(0.,1.,0.));
#7968=DIRECTION('center_axis',(0.,1.,0.));
#7969=DIRECTION('ref_axis',(0.,0.,1.));
#7970=DIRECTION('center_axis',(0.,1.,0.));
#7971=DIRECTION('ref_axis',(0.,0.,1.));
#7972=DIRECTION('',(-8.65956056235494E-17,0.707106781186548,-0.707106781186548));
#7973=DIRECTION('center_axis',(0.,-1.,0.));
#7974=DIRECTION('ref_axis',(0.,0.,-1.));
#7975=DIRECTION('center_axis',(0.,-1.,0.));
#7976=DIRECTION('ref_axis',(0.,0.,-1.));
#7977=DIRECTION('center_axis',(0.,1.,0.));
#7978=DIRECTION('ref_axis',(0.,0.,1.));
#7979=DIRECTION('',(0.,-1.,0.));
#7980=DIRECTION('axis',(0.,0.,1.));
#7981=DIRECTION('refdir',(1.,0.,0.));
#7982=DIRECTION('center_axis',(0.866025403784443,0.,0.499999999999992));
#7983=DIRECTION('ref_axis',(0.499999999999992,0.,-0.866025403784443));
#7984=DIRECTION('',(0.866025403784444,0.,0.499999999999991));
#7985=DIRECTION('center_axis',(-0.866025403784443,0.,-0.499999999999992));
#7986=DIRECTION('ref_axis',(-0.499999999999992,0.,0.866025403784443));
#7987=DIRECTION('',(0.866025403784443,0.,0.499999999999992));
#7988=DIRECTION('center_axis',(-0.866025403784443,0.,-0.499999999999992));
#7989=DIRECTION('ref_axis',(-0.499999999999992,0.,0.866025403784443));
#7990=DIRECTION('center_axis',(0.866025403784443,0.,0.499999999999992));
#7991=DIRECTION('ref_axis',(0.499999999999992,0.,-0.866025403784443));
#7992=DIRECTION('',(0.866025403784443,0.,0.499999999999993));
#7993=DIRECTION('center_axis',(-0.866025403784443,0.,-0.499999999999992));
#7994=DIRECTION('ref_axis',(-0.499999999999992,0.,0.866025403784443));
#7995=DIRECTION('',(0.866025403784443,0.,0.499999999999993));
#7996=DIRECTION('center_axis',(-0.866025403784443,0.,-0.499999999999992));
#7997=DIRECTION('ref_axis',(-0.499999999999992,0.,0.866025403784443));
#7998=DIRECTION('center_axis',(0.866025403784443,0.,0.499999999999992));
#7999=DIRECTION('ref_axis',(0.499999999999992,0.,-0.866025403784443));
#8000=DIRECTION('center_axis',(-0.866025403784443,0.,-0.499999999999992));
#8001=DIRECTION('ref_axis',(-0.499999999999992,0.,0.866025403784443));
#8002=DIRECTION('',(0.866025403784443,0.,0.499999999999992));
#8003=DIRECTION('center_axis',(-0.866025403784443,0.,-0.499999999999992));
#8004=DIRECTION('ref_axis',(-0.499999999999992,0.,0.866025403784443));
#8005=DIRECTION('',(0.866025403784443,0.,0.499999999999992));
#8006=DIRECTION('center_axis',(0.866025403784443,0.,0.499999999999992));
#8007=DIRECTION('ref_axis',(0.499999999999992,0.,-0.866025403784443));
#8008=DIRECTION('',(0.866025403784443,0.,0.499999999999992));
#8009=DIRECTION('',(0.866025403784443,0.,0.499999999999992));
#8010=DIRECTION('center_axis',(0.866025403784443,0.,0.499999999999992));
#8011=DIRECTION('ref_axis',(0.499999999999992,0.,-0.866025403784443));
#8012=DIRECTION('',(0.866025403784443,0.,0.499999999999992));
#8013=DIRECTION('',(0.866025403784443,0.,0.499999999999992));
#8014=DIRECTION('center_axis',(0.866025403784443,0.,0.499999999999992));
#8015=DIRECTION('ref_axis',(0.499999999999992,0.,-0.866025403784443));
#8016=DIRECTION('',(0.866025403784444,0.,0.499999999999991));
#8017=DIRECTION('',(0.866025403784443,0.,0.499999999999992));
#8018=DIRECTION('center_axis',(0.866025403784443,0.,0.499999999999992));
#8019=DIRECTION('ref_axis',(0.499999999999992,0.,-0.866025403784443));
#8020=DIRECTION('',(0.866025403784443,0.,0.499999999999993));
#8021=DIRECTION('',(0.866025403784443,0.,0.499999999999992));
#8022=DIRECTION('center_axis',(0.866025403784443,0.,0.499999999999992));
#8023=DIRECTION('ref_axis',(0.499999999999992,0.,-0.866025403784443));
#8024=DIRECTION('center_axis',(-0.866025403784443,0.,-0.499999999999992));
#8025=DIRECTION('ref_axis',(-0.499999999999992,0.,0.866025403784443));
#8026=DIRECTION('',(0.866025403784443,0.,0.499999999999992));
#8027=DIRECTION('center_axis',(-0.866025403784443,0.,-0.499999999999992));
#8028=DIRECTION('ref_axis',(-0.499999999999992,0.,0.866025403784443));
#8029=DIRECTION('',(0.866025403784443,0.,0.499999999999992));
#8030=DIRECTION('center_axis',(0.866025403784443,0.,0.499999999999992));
#8031=DIRECTION('ref_axis',(0.499999999999992,0.,-0.866025403784443));
#8032=DIRECTION('',(0.866025403784443,0.,0.499999999999992));
#8033=DIRECTION('',(0.866025403784443,0.,0.499999999999993));
#8034=DIRECTION('center_axis',(0.866025403784443,0.,0.499999999999992));
#8035=DIRECTION('ref_axis',(0.499999999999992,0.,-0.866025403784443));
#8036=DIRECTION('',(0.866025403784444,0.,0.499999999999991));
#8037=DIRECTION('',(0.866025403784443,0.,0.499999999999992));
#8038=DIRECTION('center_axis',(0.866025403784443,0.,0.499999999999992));
#8039=DIRECTION('ref_axis',(0.499999999999992,0.,-0.866025403784443));
#8040=DIRECTION('',(0.866025403784443,0.,0.499999999999992));
#8041=DIRECTION('',(0.866025403784443,0.,0.499999999999992));
#8042=DIRECTION('center_axis',(0.866025403784443,0.,0.499999999999992));
#8043=DIRECTION('ref_axis',(0.499999999999992,0.,-0.866025403784443));
#8044=DIRECTION('',(0.866025403784444,0.,0.49999999999999));
#8045=DIRECTION('',(0.866025403784441,0.,0.499999999999995));
#8046=DIRECTION('center_axis',(0.866025403784443,0.,0.499999999999992));
#8047=DIRECTION('ref_axis',(0.499999999999992,0.,-0.866025403784443));
#8048=DIRECTION('',(0.866025403784443,0.,0.499999999999993));
#8049=DIRECTION('',(0.866025403784443,0.,0.499999999999992));
#8050=DIRECTION('center_axis',(0.866025403784443,0.,0.499999999999992));
#8051=DIRECTION('ref_axis',(0.499999999999992,0.,-0.866025403784443));
#8052=DIRECTION('',(0.866025403784443,0.,0.499999999999992));
#8053=DIRECTION('',(0.866025403784443,0.,0.499999999999992));
#8054=DIRECTION('center_axis',(0.866025403784443,0.,0.499999999999992));
#8055=DIRECTION('ref_axis',(0.499999999999992,0.,-0.866025403784443));
#8056=DIRECTION('',(0.866025403784443,0.,0.499999999999992));
#8057=DIRECTION('',(0.866025403784443,0.,0.499999999999992));
#8058=DIRECTION('center_axis',(0.866025403784443,0.,0.499999999999992));
#8059=DIRECTION('ref_axis',(0.499999999999992,0.,-0.866025403784443));
#8060=DIRECTION('',(0.866025403784443,0.,0.499999999999992));
#8061=DIRECTION('',(0.866025403784444,0.,0.499999999999991));
#8062=DIRECTION('center_axis',(0.866025403784443,0.,0.499999999999992));
#8063=DIRECTION('ref_axis',(-0.433012701892211,0.500000000000004,0.750000000000002));
#8064=DIRECTION('center_axis',(-0.866025403784443,0.,-0.499999999999992));
#8065=DIRECTION('ref_axis',(-0.499999999999992,0.,0.866025403784443));
#8066=DIRECTION('',(0.866025403784443,0.,0.499999999999992));
#8067=DIRECTION('center_axis',(-0.866025403784443,0.,-0.499999999999992));
#8068=DIRECTION('ref_axis',(-0.499999999999992,0.,0.866025403784443));
#8069=DIRECTION('',(0.866025403784443,0.,0.499999999999992));
#8070=DIRECTION('center_axis',(0.866025403784443,0.,0.499999999999992));
#8071=DIRECTION('ref_axis',(-0.433012701892234,0.499999999999926,0.750000000000041));
#8072=DIRECTION('',(0.866025403784443,0.,0.499999999999992));
#8073=DIRECTION('center_axis',(-0.866025403784443,0.,-0.499999999999992));
#8074=DIRECTION('ref_axis',(-0.499999999999992,0.,0.866025403784443));
#8075=DIRECTION('',(0.866025403784442,0.,0.499999999999994));
#8076=DIRECTION('center_axis',(-0.866025403784443,0.,-0.499999999999992));
#8077=DIRECTION('ref_axis',(-0.499999999999992,0.,0.866025403784443));
#8078=DIRECTION('center_axis',(-0.866025403784443,0.,-0.499999999999992));
#8079=DIRECTION('ref_axis',(-0.499999999999992,0.,0.866025403784443));
#8080=DIRECTION('center_axis',(-0.866025403784443,0.,-0.499999999999992));
#8081=DIRECTION('ref_axis',(-0.499999999999992,0.,0.866025403784443));
#8082=DIRECTION('',(-0.433012701892229,-0.499999999999983,0.750000000000006));
#8083=DIRECTION('center_axis',(0.866025403784443,-2.25118642417821E-16,
0.499999999999992));
#8084=DIRECTION('ref_axis',(0.499999999999992,0.,-0.866025403784443));
#8085=DIRECTION('',(-0.433012701892221,-0.499999999999992,0.750000000000004));
#8086=DIRECTION('',(0.433012701892197,-0.500000000000028,-0.749999999999994));
#8087=DIRECTION('center_axis',(0.866025403784443,2.4704687096211E-16,0.499999999999992));
#8088=DIRECTION('ref_axis',(0.499999999999992,0.,-0.866025403784443));
#8089=DIRECTION('',(0.433012701892204,-0.500000000000004,-0.750000000000006));
#8090=DIRECTION('',(0.,1.,0.));
#8091=DIRECTION('center_axis',(0.866025403784443,0.,0.499999999999992));
#8092=DIRECTION('ref_axis',(0.499999999999992,0.,-0.866025403784443));
#8093=DIRECTION('',(0.,1.,0.));
#8094=DIRECTION('center_axis',(-0.866025403784443,0.,-0.499999999999992));
#8095=DIRECTION('ref_axis',(-0.499999999999992,0.,0.866025403784443));
#8096=DIRECTION('center_axis',(-0.866025403784443,0.,-0.499999999999992));
#8097=DIRECTION('ref_axis',(-0.499999999999992,0.,0.866025403784443));
#8098=DIRECTION('',(-0.43301270189221,0.500000000000002,0.750000000000004));
#8099=DIRECTION('',(0.25,0.866025403784439,-0.433012701892219));
#8100=DIRECTION('',(0.433012701892205,-0.500000000000012,-0.75));
#8101=DIRECTION('',(0.433012701892215,0.499999999999987,-0.750000000000011));
#8102=DIRECTION('',(0.25,-0.86602540378444,-0.433012701892216));
#8103=DIRECTION('',(-0.433012701892207,-0.499999999999993,0.750000000000012));
#8104=DIRECTION('',(0.,-1.,0.));
#8105=DIRECTION('',(-0.499999999999994,0.,0.866025403784442));
#8106=DIRECTION('',(0.,1.,0.));
#8107=DIRECTION('center_axis',(0.866025403784443,0.,0.499999999999992));
#8108=DIRECTION('ref_axis',(0.499999999999992,0.,-0.866025403784443));
#8109=DIRECTION('',(-0.866025403784443,0.,-0.499999999999992));
#8110=DIRECTION('center_axis',(-0.866025403784443,0.,-0.499999999999992));
#8111=DIRECTION('ref_axis',(-0.499999999999992,0.,0.866025403784443));
#8112=DIRECTION('',(0.433012701892209,-0.500000000000007,-0.750000000000001));
#8113=DIRECTION('',(0.250000000000001,0.866025403784442,-0.433012701892212));
#8114=DIRECTION('',(-0.433012701892215,0.499999999999997,0.750000000000005));
#8115=DIRECTION('',(0.,1.,0.));
#8116=DIRECTION('',(-0.499999999999994,0.,0.866025403784442));
#8117=DIRECTION('',(0.,-1.,0.));
#8118=DIRECTION('',(-0.433012701892214,-0.499999999999991,0.750000000000009));
#8119=DIRECTION('',(0.249999999999992,-0.866025403784442,-0.433012701892217));
#8120=DIRECTION('',(0.433012701892219,0.499999999999982,-0.750000000000012));
#8121=DIRECTION('center_axis',(0.866025403784443,0.,0.499999999999992));
#8122=DIRECTION('ref_axis',(0.499999999999992,0.,-0.866025403784443));
#8123=DIRECTION('center_axis',(-0.866025403784443,0.,-0.499999999999992));
#8124=DIRECTION('ref_axis',(-0.499999999999992,0.,0.866025403784443));
#8125=DIRECTION('',(-0.433012701892211,-0.49999999999998,0.750000000000018));
#8126=DIRECTION('center_axis',(-0.866025403784443,0.,-0.499999999999992));
#8127=DIRECTION('ref_axis',(-0.499999999999992,0.,0.866025403784443));
#8128=DIRECTION('',(0.433012701892242,0.49999999999998,-0.750000000000001));
#8129=DIRECTION('',(0.,1.,0.));
#8130=DIRECTION('center_axis',(-0.866025403784443,0.,-0.499999999999992));
#8131=DIRECTION('ref_axis',(-0.499999999999992,0.,0.866025403784443));
#8132=DIRECTION('',(0.,-1.,0.));
#8133=DIRECTION('',(0.433012701892204,-0.500000000000004,-0.750000000000006));
#8134=DIRECTION('center_axis',(-0.866025403784443,0.,-0.499999999999992));
#8135=DIRECTION('ref_axis',(-0.499999999999992,0.,0.866025403784443));
#8136=DIRECTION('',(-0.433012701892195,0.499999999999999,0.750000000000015));
#8137=DIRECTION('center_axis',(0.,-1.,0.));
#8138=DIRECTION('ref_axis',(0.,0.,-1.));
#8139=DIRECTION('center_axis',(0.,-1.,0.));
#8140=DIRECTION('ref_axis',(0.,0.,-1.));
#8141=DIRECTION('center_axis',(0.,1.,0.));
#8142=DIRECTION('ref_axis',(0.,0.,1.));
#8143=DIRECTION('center_axis',(0.,1.,0.));
#8144=DIRECTION('ref_axis',(0.,0.,1.));
#8145=DIRECTION('',(0.,-1.,0.));
#8146=DIRECTION('',(0.,1.,0.));
#8147=DIRECTION('',(0.,1.,0.));
#8148=DIRECTION('center_axis',(0.224143868042018,-0.965925826289067,0.129409522551263));
#8149=DIRECTION('ref_axis',(0.,-0.132788176096111,-0.991144439670156));
#8150=DIRECTION('center_axis',(0.224143868042018,-0.965925826289067,0.129409522551263));
#8151=DIRECTION('ref_axis',(0.974116947696296,0.22604462437946,0.));
#8152=DIRECTION('center_axis',(-0.224143868042018,0.965925826289067,-0.129409522551263));
#8153=DIRECTION('ref_axis',(-0.974116947696296,-0.22604462437946,0.));
#8154=DIRECTION('center_axis',(-0.224143868042018,0.965925826289067,-0.129409522551263));
#8155=DIRECTION('ref_axis',(-0.974116947696296,-0.22604462437946,0.));
#8156=DIRECTION('',(0.224143868042018,-0.965925826289067,0.129409522551263));
#8157=DIRECTION('center_axis',(0.433012701892223,-0.866025403784436,0.250000000000002));
#8158=DIRECTION('ref_axis',(0.5,0.,-0.866025403784439));
#8159=DIRECTION('center_axis',(0.433012701892223,-0.866025403784436,0.250000000000002));
#8160=DIRECTION('ref_axis',(0.894427190999914,0.447213595499962,0.));
#8161=DIRECTION('center_axis',(-0.433012701892223,0.866025403784436,-0.250000000000002));
#8162=DIRECTION('ref_axis',(-0.894427190999914,-0.447213595499962,0.));
#8163=DIRECTION('center_axis',(-0.433012701892223,0.866025403784436,-0.250000000000002));
#8164=DIRECTION('ref_axis',(-0.894427190999914,-0.447213595499962,0.));
#8165=DIRECTION('',(0.433012701892223,-0.866025403784437,0.250000000000002));
#8166=DIRECTION('center_axis',(0.612372435695796,-0.707106781186546,0.353553390593275));
#8167=DIRECTION('ref_axis',(0.5,0.,-0.866025403784438));
#8168=DIRECTION('center_axis',(0.612372435695796,-0.707106781186546,0.353553390593275));
#8169=DIRECTION('ref_axis',(0.755928946018453,0.654653670707979,0.));
#8170=DIRECTION('center_axis',(-0.612372435695796,0.707106781186546,-0.353553390593275));
#8171=DIRECTION('ref_axis',(-0.755928946018453,-0.654653670707979,0.));
#8172=DIRECTION('center_axis',(-0.612372435695796,0.707106781186546,-0.353553390593275));
#8173=DIRECTION('ref_axis',(-0.755928946018453,-0.654653670707979,0.));
#8174=DIRECTION('',(0.612372435695796,-0.707106781186546,0.353553390593275));
#8175=DIRECTION('center_axis',(0.,1.,0.));
#8176=DIRECTION('ref_axis',(0.,0.,1.));
#8177=DIRECTION('center_axis',(0.,1.,0.));
#8178=DIRECTION('ref_axis',(0.,0.,1.));
#8179=DIRECTION('center_axis',(0.,1.,0.));
#8180=DIRECTION('ref_axis',(0.,0.,1.));
#8181=DIRECTION('center_axis',(0.,1.,0.));
#8182=DIRECTION('ref_axis',(0.,0.,1.));
#8183=DIRECTION('',(0.,1.,0.));
#8184=DIRECTION('center_axis',(-0.224143868042018,0.965925826289067,-0.129409522551263));
#8185=DIRECTION('ref_axis',(0.,0.132788176096111,0.991144439670156));
#8186=DIRECTION('center_axis',(-0.224143868042018,0.965925826289067,-0.129409522551263));
#8187=DIRECTION('ref_axis',(-0.974116947696296,-0.22604462437946,0.));
#8188=DIRECTION('center_axis',(-0.224143868042018,0.965925826289067,-0.129409522551263));
#8189=DIRECTION('ref_axis',(-0.974116947696296,-0.22604462437946,0.));
#8190=DIRECTION('center_axis',(-0.224143868042018,0.965925826289067,-0.129409522551263));
#8191=DIRECTION('ref_axis',(-0.974116947696296,-0.22604462437946,0.));
#8192=DIRECTION('',(-0.224143868042018,0.965925826289067,-0.129409522551263));
#8193=DIRECTION('center_axis',(-0.433012701892223,0.866025403784436,-0.250000000000002));
#8194=DIRECTION('ref_axis',(-0.499999999999999,0.,0.866025403784439));
#8195=DIRECTION('center_axis',(-0.433012701892223,0.866025403784436,-0.250000000000002));
#8196=DIRECTION('ref_axis',(-0.894427190999914,-0.447213595499962,0.));
#8197=DIRECTION('center_axis',(-0.433012701892223,0.866025403784436,-0.250000000000002));
#8198=DIRECTION('ref_axis',(-0.894427190999914,-0.447213595499962,0.));
#8199=DIRECTION('center_axis',(-0.433012701892223,0.866025403784436,-0.250000000000002));
#8200=DIRECTION('ref_axis',(-0.894427190999914,-0.447213595499962,0.));
#8201=DIRECTION('',(-0.433012701892223,0.866025403784436,-0.250000000000002));
#8202=DIRECTION('center_axis',(0.866025403784443,0.,0.499999999999992));
#8203=DIRECTION('ref_axis',(0.499999999999992,0.,-0.866025403784443));
#8204=DIRECTION('center_axis',(-0.866025403784443,0.,-0.499999999999992));
#8205=DIRECTION('ref_axis',(-0.499999999999992,0.,0.866025403784443));
#8206=DIRECTION('',(0.866025403784443,0.,0.499999999999992));
#8207=DIRECTION('center_axis',(-0.866025403784443,0.,-0.499999999999992));
#8208=DIRECTION('ref_axis',(-0.499999999999992,0.,0.866025403784443));
#8209=DIRECTION('center_axis',(-0.612372435695796,0.707106781186546,-0.353553390593275));
#8210=DIRECTION('ref_axis',(-0.5,0.,0.866025403784438));
#8211=DIRECTION('center_axis',(-0.612372435695796,0.707106781186546,-0.353553390593275));
#8212=DIRECTION('ref_axis',(-0.755928946018453,-0.654653670707979,0.));
#8213=DIRECTION('center_axis',(-0.612372435695796,0.707106781186546,-0.353553390593275));
#8214=DIRECTION('ref_axis',(-0.755928946018453,-0.654653670707979,0.));
#8215=DIRECTION('center_axis',(-0.612372435695796,0.707106781186546,-0.353553390593275));
#8216=DIRECTION('ref_axis',(-0.755928946018453,-0.654653670707979,0.));
#8217=DIRECTION('',(-0.612372435695796,0.707106781186546,-0.353553390593275));
#8218=DIRECTION('center_axis',(0.,1.,0.));
#8219=DIRECTION('ref_axis',(0.,0.,1.));
#8220=DIRECTION('',(0.,1.,0.));
#8221=DIRECTION('center_axis',(-0.224143868042018,0.965925826289067,-0.129409522551263));
#8222=DIRECTION('ref_axis',(-0.974116947696296,-0.22604462437946,0.));
#8223=DIRECTION('',(-0.224143868042018,0.965925826289067,-0.129409522551263));
#8224=DIRECTION('center_axis',(-0.433012701892223,0.866025403784437,-0.250000000000002));
#8225=DIRECTION('ref_axis',(-0.894427190999914,-0.447213595499962,0.));
#8226=DIRECTION('',(-0.433012701892223,0.866025403784436,-0.250000000000002));
#8227=DIRECTION('center_axis',(-0.612372435695796,0.707106781186546,-0.353553390593275));
#8228=DIRECTION('ref_axis',(-0.755928946018453,-0.654653670707979,0.));
#8229=DIRECTION('',(-0.612372435695796,0.707106781186546,-0.353553390593275));
#8230=DIRECTION('center_axis',(0.433012701892215,0.499999999999992,-0.750000000000008));
#8231=DIRECTION('ref_axis',(-0.866025403784443,0.,-0.499999999999992));
#8232=DIRECTION('center_axis',(0.433012701892215,0.499999999999992,-0.750000000000008));
#8233=DIRECTION('ref_axis',(-0.649519052838319,0.750000000000008,0.125000000000006));
#8234=DIRECTION('center_axis',(-0.433012701892215,-0.499999999999992,0.750000000000008));
#8235=DIRECTION('ref_axis',(0.649519052838319,-0.750000000000008,-0.125000000000006));
#8236=DIRECTION('center_axis',(-0.433012701892215,-0.499999999999992,0.750000000000008));
#8237=DIRECTION('ref_axis',(0.649519052838319,-0.750000000000008,-0.125000000000006));
#8238=DIRECTION('',(0.433012701892215,0.499999999999992,-0.750000000000008));
#8239=DIRECTION('',(-0.433012701892199,-0.500000000000005,0.750000000000008));
#8240=DIRECTION('',(-0.433012701892214,-0.499999999999978,0.750000000000018));
#8241=DIRECTION('center_axis',(-0.433012701892211,0.500000000000004,0.750000000000002));
#8242=DIRECTION('ref_axis',(0.866025403784443,0.,0.499999999999992));
#8243=DIRECTION('center_axis',(-0.433012701892211,0.500000000000004,0.750000000000002));
#8244=DIRECTION('ref_axis',(-0.649519052838324,-0.750000000000002,0.125000000000015));
#8245=DIRECTION('center_axis',(0.433012701892211,-0.500000000000004,-0.750000000000002));
#8246=DIRECTION('ref_axis',(0.649519052838324,0.750000000000002,-0.125000000000015));
#8247=DIRECTION('center_axis',(0.433012701892211,-0.500000000000004,-0.750000000000002));
#8248=DIRECTION('ref_axis',(0.649519052838324,0.750000000000002,-0.125000000000015));
#8249=DIRECTION('',(-0.433012701892211,0.500000000000004,0.750000000000002));
#8250=DIRECTION('',(0.433012701892208,-0.499999999999987,-0.750000000000015));
#8251=DIRECTION('',(0.433012701892233,-0.50000000000002,-0.749999999999979));
#8252=DIRECTION('center_axis',(0.642402019910919,0.482962913144524,-0.595034847165548));
#8253=DIRECTION('ref_axis',(-0.679542161318994,0.,-0.733636456966194));
#8254=DIRECTION('center_axis',(0.642402019910919,0.482962913144524,-0.595034847165548));
#8255=DIRECTION('ref_axis',(0.510942898759438,0.308782699291242,0.802240985506049));
#8256=DIRECTION('center_axis',(-0.642402019910919,-0.482962913144524,0.595034847165548));
#8257=DIRECTION('ref_axis',(-0.510942898759438,-0.308782699291242,-0.802240985506049));
#8258=DIRECTION('center_axis',(-0.642402019910919,-0.482962913144524,0.595034847165548));
#8259=DIRECTION('ref_axis',(-0.510942898759438,-0.308782699291242,-0.802240985506049));
#8260=DIRECTION('',(0.642402019910919,0.482962913144524,-0.595034847165548));
#8261=DIRECTION('center_axis',(-0.194114283826876,0.482962913144539,0.853853892268062));
#8262=DIRECTION('ref_axis',(0.975118889534635,0.,0.221682546161714));
#8263=DIRECTION('center_axis',(-0.194114283826876,0.482962913144539,0.853853892268062));
#8264=DIRECTION('ref_axis',(0.706703285860956,-0.534827323670698,0.463174048936862));
#8265=DIRECTION('center_axis',(0.194114283826876,-0.482962913144539,-0.853853892268062));
#8266=DIRECTION('ref_axis',(-0.706703285860956,0.534827323670698,-0.463174048936862));
#8267=DIRECTION('center_axis',(0.194114283826876,-0.482962913144539,-0.853853892268062));
#8268=DIRECTION('ref_axis',(-0.706703285860956,0.534827323670698,-0.463174048936862));
#8269=DIRECTION('',(-0.194114283826876,0.482962913144539,0.853853892268062));
#8270=DIRECTION('center_axis',(0.808012701892221,0.433012701892207,-0.399519052838338));
#8271=DIRECTION('ref_axis',(-0.443226594010285,0.,-0.89640960858418));
#8272=DIRECTION('center_axis',(0.808012701892221,0.433012701892207,-0.399519052838338));
#8273=DIRECTION('ref_axis',(0.365367827064589,0.163691536870759,0.916357698556077));
#8274=DIRECTION('center_axis',(-0.808012701892221,-0.433012701892208,0.399519052838338));
#8275=DIRECTION('ref_axis',(-0.365367827064589,-0.163691536870759,-0.916357698556077));
#8276=DIRECTION('center_axis',(-0.808012701892221,-0.433012701892207,0.399519052838338));
#8277=DIRECTION('ref_axis',(-0.365367827064589,-0.163691536870759,-0.916357698556077));
#8278=DIRECTION('',(0.808012701892221,0.433012701892207,-0.399519052838338));
#8279=DIRECTION('center_axis',(0.058012701892234,0.433012701892226,0.899519052838325));
#8280=DIRECTION('ref_axis',(0.997926790235505,0.,-0.064359314246356));
#8281=DIRECTION('center_axis',(0.058012701892234,0.433012701892226,0.899519052838325));
#8282=DIRECTION('ref_axis',(0.752666161685325,-0.610905132370716,0.245537305306135));
#8283=DIRECTION('center_axis',(-0.0580127018922341,-0.433012701892225,-0.899519052838325));
#8284=DIRECTION('ref_axis',(-0.752666161685325,0.610905132370716,-0.245537305306135));
#8285=DIRECTION('center_axis',(-0.058012701892234,-0.433012701892226,-0.899519052838325));
#8286=DIRECTION('ref_axis',(-0.752666161685325,0.610905132370716,-0.245537305306135));
#8287=DIRECTION('',(0.058012701892234,0.433012701892226,0.899519052838325));
#8288=DIRECTION('center_axis',(0.918558653543694,0.353553390593261,-0.176776695296649));
#8289=DIRECTION('ref_axis',(-0.188982236504625,0.,-0.981980506061963));
#8290=DIRECTION('center_axis',(0.918558653543694,0.353553390593261,-0.176776695296649));
#8291=DIRECTION('ref_axis',(0.188982236504626,0.,0.981980506061964));
#8292=DIRECTION('center_axis',(-0.918558653543694,-0.353553390593261,0.176776695296649));
#8293=DIRECTION('ref_axis',(-0.188982236504626,-5.55111512312578E-17,-0.981980506061963));
#8294=DIRECTION('center_axis',(-0.918558653543694,-0.353553390593261,0.176776695296649));
#8295=DIRECTION('ref_axis',(-0.188982236504626,0.,-0.981980506061964));
#8296=DIRECTION('',(0.918558653543694,0.353553390593261,-0.176776695296649));
#8297=DIRECTION('center_axis',(0.30618621784791,0.353553390593282,0.883883476483177));
#8298=DIRECTION('ref_axis',(0.944911182523063,0.,-0.327326835354004));
#8299=DIRECTION('center_axis',(0.30618621784791,0.353553390593282,0.883883476483177));
#8300=DIRECTION('ref_axis',(0.755928946018457,-0.654653670707974,-7.66053886991358E-15));
#8301=DIRECTION('center_axis',(-0.30618621784791,-0.353553390593282,-0.883883476483177));
#8302=DIRECTION('ref_axis',(-0.755928946018457,0.654653670707974,7.60502771868232E-15));
#8303=DIRECTION('center_axis',(-0.30618621784791,-0.353553390593282,-0.883883476483177));
#8304=DIRECTION('ref_axis',(-0.755928946018457,0.654653670707974,7.66053886991358E-15));
#8305=DIRECTION('',(0.30618621784791,0.353553390593282,0.883883476483177));
#8306=DIRECTION('center_axis',(0.433012701892215,-0.499999999999992,-0.750000000000008));
#8307=DIRECTION('ref_axis',(0.649519052838319,0.750000000000008,-0.125000000000006));
#8308=DIRECTION('',(0.433012701892215,-0.499999999999992,-0.750000000000008));
#8309=DIRECTION('center_axis',(0.433012701892211,-0.500000000000004,-0.750000000000002));
#8310=DIRECTION('ref_axis',(0.,0.832050294337842,-0.554700196225231));
#8311=DIRECTION('center_axis',(-0.433012701892211,-0.500000000000004,0.750000000000002));
#8312=DIRECTION('ref_axis',(0.649519052838324,-0.750000000000002,-0.125000000000015));
#8313=DIRECTION('',(-0.433012701892211,-0.500000000000004,0.750000000000002));
#8314=DIRECTION('center_axis',(-0.433012701892215,-0.499999999999992,0.750000000000008));
#8315=DIRECTION('ref_axis',(0.,-0.832050294337851,-0.554700196225219));
#8316=DIRECTION('center_axis',(0.194114283826879,-0.482962913144528,-0.853853892268068));
#8317=DIRECTION('ref_axis',(-0.70670328586096,0.534827323670699,-0.463174048936855));
#8318=DIRECTION('',(0.194114283826879,-0.482962913144527,-0.853853892268068));
#8319=DIRECTION('center_axis',(0.194114283826876,-0.482962913144539,-0.853853892268062));
#8320=DIRECTION('ref_axis',(0.,0.87041002959648,-0.492327513326093));
#8321=DIRECTION('center_axis',(-0.642402019910915,-0.482962913144535,0.595034847165542));
#8322=DIRECTION('ref_axis',(-0.510942898759436,-0.308782699291236,-0.802240985506053));
#8323=DIRECTION('',(-0.642402019910915,-0.482962913144535,0.595034847165542));
#8324=DIRECTION('center_axis',(-0.642402019910919,-0.482962913144524,0.595034847165548));
#8325=DIRECTION('ref_axis',(0.679542161318994,0.,0.733636456966194));
#8326=DIRECTION('center_axis',(-0.0580127018922311,-0.433012701892215,-0.89951905283833));
#8327=DIRECTION('ref_axis',(-0.752666161685329,0.610905132370714,-0.245537305306127));
#8328=DIRECTION('',(-0.0580127018922311,-0.433012701892215,-0.89951905283833));
#8329=DIRECTION('center_axis',(-0.0580127018922341,-0.433012701892225,-0.899519052838325));
#8330=DIRECTION('ref_axis',(0.,0.901036538010451,-0.433743192649915));
#8331=DIRECTION('center_axis',(-0.808012701892218,-0.433012701892218,0.399519052838333));
#8332=DIRECTION('ref_axis',(-0.365367827064587,-0.163691536870751,-0.916357698556079));
#8333=DIRECTION('',(-0.808012701892218,-0.433012701892218,0.399519052838333));
#8334=DIRECTION('center_axis',(-0.808012701892221,-0.433012701892208,0.399519052838338));
#8335=DIRECTION('ref_axis',(0.472347490483135,-0.881412416655384,0.));
#8336=DIRECTION('center_axis',(-0.306186217847908,-0.353553390593273,-0.883883476483181));
#8337=DIRECTION('ref_axis',(-0.755928946018462,0.654653670707968,1.58761892521397E-14));
#8338=DIRECTION('',(-0.306186217847908,-0.353553390593273,-0.883883476483181));
#8339=DIRECTION('center_axis',(-0.30618621784791,-0.353553390593282,-0.883883476483177));
#8340=DIRECTION('ref_axis',(0.,0.928476690885255,-0.371390676354114));
#8341=DIRECTION('center_axis',(-0.918558653543692,-0.35355339059327,0.176776695296645));
#8342=DIRECTION('ref_axis',(-0.188982236504625,1.0547118733939E-14,-0.981980506061964));
#8343=DIRECTION('',(-0.918558653543692,-0.35355339059327,0.176776695296645));
#8344=DIRECTION('center_axis',(-0.918558653543694,-0.353553390593261,0.176776695296649));
#8345=DIRECTION('ref_axis',(0.359210604053538,-0.933256525257387,0.));
#8346=DIRECTION('center_axis',(-0.433012701892215,-0.499999999999992,0.750000000000008));
#8347=DIRECTION('ref_axis',(0.866025403784443,0.,0.499999999999992));
#8348=DIRECTION('center_axis',(-0.433012701892215,-0.499999999999992,0.750000000000008));
#8349=DIRECTION('ref_axis',(0.649519052838319,-0.750000000000008,-0.125000000000006));
#8350=DIRECTION('center_axis',(-0.433012701892215,-0.499999999999992,0.750000000000008));
#8351=DIRECTION('ref_axis',(0.649519052838319,-0.750000000000008,-0.125000000000006));
#8352=DIRECTION('',(-0.433012701892215,-0.499999999999992,0.750000000000008));
#8353=DIRECTION('center_axis',(0.433012701892211,-0.500000000000004,-0.750000000000002));
#8354=DIRECTION('ref_axis',(-0.866025403784443,0.,-0.499999999999992));
#8355=DIRECTION('center_axis',(0.433012701892211,-0.500000000000004,-0.750000000000002));
#8356=DIRECTION('ref_axis',(0.649519052838324,0.750000000000002,-0.125000000000015));
#8357=DIRECTION('center_axis',(0.433012701892211,-0.500000000000004,-0.750000000000002));
#8358=DIRECTION('ref_axis',(0.649519052838324,0.750000000000002,-0.125000000000015));
#8359=DIRECTION('',(0.433012701892211,-0.500000000000004,-0.750000000000002));
#8360=DIRECTION('center_axis',(-0.642402019910919,-0.482962913144524,0.595034847165548));
#8361=DIRECTION('ref_axis',(0.679542161318994,0.,0.733636456966194));
#8362=DIRECTION('center_axis',(-0.642402019910919,-0.482962913144524,0.595034847165548));
#8363=DIRECTION('ref_axis',(-0.510942898759438,-0.308782699291242,-0.802240985506049));
#8364=DIRECTION('center_axis',(-0.642402019910919,-0.482962913144524,0.595034847165548));
#8365=DIRECTION('ref_axis',(-0.510942898759438,-0.308782699291242,-0.802240985506049));
#8366=DIRECTION('',(-0.642402019910919,-0.482962913144524,0.595034847165548));
#8367=DIRECTION('center_axis',(0.194114283826876,-0.482962913144539,-0.853853892268062));
#8368=DIRECTION('ref_axis',(-0.975118889534635,0.,-0.221682546161714));
#8369=DIRECTION('center_axis',(0.194114283826876,-0.482962913144539,-0.853853892268062));
#8370=DIRECTION('ref_axis',(-0.706703285860956,0.534827323670698,-0.463174048936862));
#8371=DIRECTION('center_axis',(0.194114283826876,-0.482962913144539,-0.853853892268062));
#8372=DIRECTION('ref_axis',(-0.706703285860956,0.534827323670698,-0.463174048936862));
#8373=DIRECTION('',(0.194114283826876,-0.482962913144539,-0.853853892268062));
#8374=DIRECTION('center_axis',(-0.808012701892221,-0.433012701892208,0.399519052838338));
#8375=DIRECTION('ref_axis',(0.443226594010285,0.,0.89640960858418));
#8376=DIRECTION('center_axis',(-0.808012701892221,-0.433012701892208,0.399519052838338));
#8377=DIRECTION('ref_axis',(-0.365367827064589,-0.163691536870759,-0.916357698556077));
#8378=DIRECTION('center_axis',(-0.808012701892221,-0.433012701892207,0.399519052838338));
#8379=DIRECTION('ref_axis',(-0.365367827064589,-0.163691536870759,-0.916357698556077));
#8380=DIRECTION('',(-0.808012701892221,-0.433012701892207,0.399519052838338));
#8381=DIRECTION('center_axis',(-0.0580127018922341,-0.433012701892225,-0.899519052838325));
#8382=DIRECTION('ref_axis',(-0.997926790235505,0.,0.0643593142463562));
#8383=DIRECTION('center_axis',(-0.0580127018922341,-0.433012701892225,-0.899519052838325));
#8384=DIRECTION('ref_axis',(-0.752666161685325,0.610905132370716,-0.245537305306135));
#8385=DIRECTION('center_axis',(-0.0580127018922342,-0.433012701892225,-0.899519052838325));
#8386=DIRECTION('ref_axis',(-0.752666161685325,0.610905132370716,-0.245537305306135));
#8387=DIRECTION('',(-0.0580127018922342,-0.433012701892225,-0.899519052838325));
#8388=DIRECTION('center_axis',(-0.918558653543694,-0.353553390593261,0.176776695296649));
#8389=DIRECTION('ref_axis',(0.188982236504625,0.,0.981980506061963));
#8390=DIRECTION('center_axis',(-0.918558653543694,-0.353553390593261,0.176776695296649));
#8391=DIRECTION('ref_axis',(-0.188982236504626,-5.55111512312578E-17,-0.981980506061963));
#8392=DIRECTION('center_axis',(-0.918558653543694,-0.353553390593261,0.176776695296649));
#8393=DIRECTION('ref_axis',(-0.188982236504626,0.,-0.981980506061963));
#8394=DIRECTION('',(-0.918558653543694,-0.353553390593261,0.176776695296649));
#8395=DIRECTION('center_axis',(-0.30618621784791,-0.353553390593282,-0.883883476483177));
#8396=DIRECTION('ref_axis',(-0.944911182523063,0.,0.327326835354004));
#8397=DIRECTION('center_axis',(-0.30618621784791,-0.353553390593282,-0.883883476483177));
#8398=DIRECTION('ref_axis',(-0.755928946018457,0.654653670707974,7.60502771868232E-15));
#8399=DIRECTION('center_axis',(-0.306186217847911,-0.353553390593282,-0.883883476483177));
#8400=DIRECTION('ref_axis',(-0.755928946018457,0.654653670707974,7.66053886991358E-15));
#8401=DIRECTION('',(-0.30618621784791,-0.353553390593282,-0.883883476483177));
#8402=DIRECTION('center_axis',(-0.499999999999992,0.,0.866025403784443));
#8403=DIRECTION('ref_axis',(0.866025403784443,0.,0.499999999999992));
#8404=DIRECTION('',(0.866025403784443,0.,0.499999999999992));
#8405=DIRECTION('center_axis',(0.499999999999992,0.,-0.866025403784443));
#8406=DIRECTION('ref_axis',(-0.866025403784443,0.,-0.499999999999992));
#8407=DIRECTION('',(0.866025403784443,0.,0.499999999999992));
#8408=DIRECTION('center_axis',(-0.499999999999999,0.,0.866025403784439));
#8409=DIRECTION('ref_axis',(0.866025403784439,0.,0.499999999999999));
#8410=DIRECTION('',(0.,1.,0.));
#8411=DIRECTION('',(0.866025403784443,0.,0.499999999999992));
#8412=DIRECTION('center_axis',(0.499999999999999,0.,-0.866025403784439));
#8413=DIRECTION('ref_axis',(-0.866025403784439,0.,-0.499999999999999));
#8414=DIRECTION('',(0.866025403784443,0.,0.499999999999992));
#8415=DIRECTION('',(0.,1.,0.));
#8416=DIRECTION('center_axis',(0.866025403784443,0.,0.499999999999992));
#8417=DIRECTION('ref_axis',(0.499999999999992,0.,-0.866025403784443));
#8418=DIRECTION('center_axis',(0.249999999999998,0.866025403784436,-0.433012701892225));
#8419=DIRECTION('ref_axis',(-0.866025403784443,0.,-0.499999999999992));
#8420=DIRECTION('',(0.866025403784443,0.,0.499999999999992));
#8421=DIRECTION('center_axis',(-0.249999999999998,-0.866025403784436,0.433012701892225));
#8422=DIRECTION('ref_axis',(0.866025403784444,0.,0.499999999999991));
#8423=DIRECTION('',(0.866025403784443,0.,0.499999999999992));
#8424=DIRECTION('center_axis',(0.249999999999991,0.866025403784436,-0.433012701892229));
#8425=DIRECTION('ref_axis',(-0.866025403784452,0.,-0.499999999999977));
#8426=DIRECTION('',(0.433012701892214,-0.500000000000001,-0.750000000000002));
#8427=DIRECTION('',(0.866025403784443,0.,0.499999999999992));
#8428=DIRECTION('center_axis',(-0.249999999999991,-0.866025403784436,0.433012701892229));
#8429=DIRECTION('ref_axis',(0.866025403784451,0.,0.499999999999978));
#8430=DIRECTION('',(0.866025403784443,0.,0.499999999999992));
#8431=DIRECTION('',(0.433012701892241,-0.499999999999971,-0.750000000000007));
#8432=DIRECTION('center_axis',(0.866025403784443,0.,0.499999999999992));
#8433=DIRECTION('ref_axis',(0.499999999999992,0.,-0.866025403784443));
#8434=DIRECTION('center_axis',(0.249999999999992,-0.866025403784443,-0.433012701892215));
#8435=DIRECTION('ref_axis',(0.,0.447213595499952,-0.894427190999919));
#8436=DIRECTION('',(0.866025403784443,0.,0.499999999999992));
#8437=DIRECTION('center_axis',(-0.249999999999991,0.866025403784443,0.433012701892215));
#8438=DIRECTION('ref_axis',(0.,-0.447213595499952,0.894427190999919));
#8439=DIRECTION('',(0.866025403784443,0.,0.499999999999992));
#8440=DIRECTION('center_axis',(0.249999999999984,-0.866025403784443,-0.433012701892219));
#8441=DIRECTION('ref_axis',(0.,0.447213595499956,-0.894427190999917));
#8442=DIRECTION('',(-0.433012701892197,-0.499999999999982,0.750000000000025));
#8443=DIRECTION('',(0.866025403784443,0.,0.499999999999992));
#8444=DIRECTION('center_axis',(-0.249999999999985,0.866025403784443,0.433012701892219));
#8445=DIRECTION('ref_axis',(0.,-0.447213595499956,0.894427190999917));
#8446=DIRECTION('',(0.866025403784443,0.,0.499999999999992));
#8447=DIRECTION('',(-0.433012701892228,-0.49999999999999,0.750000000000002));
#8448=DIRECTION('center_axis',(0.866025403784443,0.,0.499999999999992));
#8449=DIRECTION('ref_axis',(0.499999999999992,0.,-0.866025403784443));
#8450=DIRECTION('center_axis',(-0.499999999999992,0.,0.866025403784443));
#8451=DIRECTION('ref_axis',(0.866025403784443,0.,0.499999999999992));
#8452=DIRECTION('',(0.866025403784442,0.,0.499999999999994));
#8453=DIRECTION('center_axis',(0.499999999999992,0.,-0.866025403784443));
#8454=DIRECTION('ref_axis',(-0.866025403784443,0.,-0.499999999999992));
#8455=DIRECTION('',(0.866025403784443,0.,0.499999999999992));
#8456=DIRECTION('center_axis',(0.,1.,0.));
#8457=DIRECTION('ref_axis',(0.,0.,1.));
#8458=DIRECTION('center_axis',(0.249999999999992,-0.866025403784443,-0.433012701892215));
#8459=DIRECTION('ref_axis',(0.,0.447213595499952,-0.894427190999919));
#8460=DIRECTION('',(0.866025403784443,0.,0.499999999999992));
#8461=DIRECTION('center_axis',(-0.249999999999992,0.866025403784443,0.433012701892215));
#8462=DIRECTION('ref_axis',(0.,-0.447213595499952,0.894427190999919));
#8463=DIRECTION('',(0.866025403784444,0.,0.499999999999991));
#8464=DIRECTION('center_axis',(-0.433012701892215,-0.499999999999992,0.750000000000008));
#8465=DIRECTION('ref_axis',(0.866025403784443,0.,0.499999999999992));
#8466=DIRECTION('center_axis',(0.249999999999998,0.866025403784436,-0.433012701892225));
#8467=DIRECTION('ref_axis',(-0.866025403784443,0.,-0.499999999999992));
#8468=DIRECTION('',(0.866025403784442,0.,0.499999999999994));
#8469=DIRECTION('center_axis',(-0.249999999999998,-0.866025403784436,0.433012701892225));
#8470=DIRECTION('ref_axis',(0.866025403784443,0.,0.499999999999992));
#8471=DIRECTION('',(0.866025403784442,0.,0.499999999999994));
#8472=DIRECTION('center_axis',(0.433012701892211,-0.500000000000004,-0.750000000000002));
#8473=DIRECTION('ref_axis',(-0.866025403784443,0.,-0.499999999999992));
#8474=DIRECTION('',(0.167217533390147,0.150383733180435,0.974383409814448));
#8475=DIRECTION('',(0.984017502884187,-0.0868240888334655,-0.155470677672055));
#8476=DIRECTION('',(0.203483849605909,0.433012701892223,0.878119765720802));
#8477=DIRECTION('',(0.963079135454496,-0.249999999999995,-0.0998928368414017));
#8478=DIRECTION('',(-0.582080363275103,0.706518960655588,0.402508892974643));
#8479=DIRECTION('',(0.651936057602406,0.701341065416795,-0.288270856587806));
#8480=DIRECTION('',(-0.596649370647445,0.767036804266037,-0.235932340740628));
#8481=DIRECTION('',(0.789972146757459,0.509627960744633,-0.340915457224631));
#8482=DIRECTION('',(-0.763916836935503,0.491742169115809,-0.417876423550952));
#8483=DIRECTION('',(0.644741097319294,0.554304778245636,-0.52636026658703));
#8484=DIRECTION('',(0.294594207717075,0.499967294374994,-0.814399752784157));
#8485=DIRECTION('',(0.939223802390978,0.00571878967484781,0.343257839629173));
#8486=DIRECTION('',(-0.490081390490008,-0.857180169929474,0.15831104501916));
#8487=DIRECTION('',(0.17360230876733,0.0819974747248357,0.98139627701016));
#8488=DIRECTION('',(-0.0586563478610911,0.150661209273828,-0.986843773287214));
#8489=DIRECTION('',(0.601865548531004,-0.783338540141622,-0.155365996988613));
#8490=DIRECTION('',(-0.836357327772553,-0.374481435442469,0.400337451146034));
#8491=DIRECTION('',(0.318384369676236,0.262663105372072,0.9108454787845));
#8492=DIRECTION('',(-0.367977985664953,-0.392555368823596,-0.842907162428778));
#8493=DIRECTION('',(0.629580921974141,-0.772291066116685,0.0848196432587745));
#8494=DIRECTION('',(-0.97842647478805,-0.140452579010683,0.151508106987968));
#8495=DIRECTION('',(0.0948179722037916,0.346271397002718,0.933330419393339));
#8496=DIRECTION('',(-0.678151608737242,-0.35128959010514,-0.64552770618375));
#8497=DIRECTION('',(0.433295742654717,-0.900576175248329,0.0348905713966902));
#8498=DIRECTION('',(-0.316000619316692,0.499967294375032,0.806335112187716));
#8499=DIRECTION('',(0.932239618762088,0.00571878967484657,0.361796335878312));
#8500=DIRECTION('',(-0.0107032057998375,-0.999934588749994,-0.00403232029813605));
#8501=DIRECTION('',(0.935731710576533,-0.011437579349689,0.352527087753742));
#8502=DIRECTION('',(0.0590809460749787,-0.956427038806394,0.285931392559331));
#8503=DIRECTION('',(-0.767949878123838,0.139453644869129,0.625144515789987));
#8504=DIRECTION('',(-0.229234787894715,-0.952986987044086,0.198159568387451));
#8505=DIRECTION('',(-0.169850534602201,-0.161294147915805,-0.972180535571177));
#8506=DIRECTION('',(0.913113954033195,-0.371432527927568,-0.168109440981762));
#8507=DIRECTION('',(-0.199196481327698,-0.766206404824012,0.610940673906497));
#8508=DIRECTION('',(-0.286859166301742,-0.112113716581807,0.951389685282999));
#8509=DIRECTION('',(-0.393154968093442,-0.891859763236021,-0.223641082505055));
#8510=DIRECTION('',(0.933130332940636,-0.302216001959502,0.194764652608507));
#8511=DIRECTION('',(-0.346015503883043,-0.607688027635677,0.714834618734169));
#8512=DIRECTION('',(-0.615134745310662,-0.109268186378082,0.780813491531256));
#8513=DIRECTION('',(-0.418701500042017,-0.793881300305476,-0.440955252704684));
#8514=DIRECTION('',(0.877794991511331,0.314854217943222,0.361030157079687));
#8515=DIRECTION('',(-0.123327141007974,-0.579721321493721,0.805427591839498));
#8516=DIRECTION('',(-0.763096497580773,0.436003989208249,0.477057917631026));
#8517=DIRECTION('',(-0.60881606453489,-0.732645702120754,-0.304258565579076));
#8518=DIRECTION('',(0.0849017445419746,-0.625751865977705,-0.775387835859675));
#8519=DIRECTION('',(-0.961035820553922,0.154028338049918,-0.22953305358887));
#8520=DIRECTION('',(0.662372101355139,-0.43280405039629,0.611509487503623));
#8521=DIRECTION('',(0.66655519646677,-0.0321649346198848,-0.744761429616252));
#8522=DIRECTION('',(0.148015383832084,-0.961306352400213,-0.232339284203163));
#8523=DIRECTION('',(-0.941595726207805,-0.0651287879951677,-0.330387241523454));
#8524=DIRECTION('',(0.176793842313733,-0.840156581135192,0.512719081461938));
#8525=DIRECTION('',(0.755486964539162,-0.218053168622206,-0.617812481312266));
#8526=DIRECTION('',(0.359299279499474,-0.388611455930554,-0.848460467005207));
#8527=DIRECTION('',(-0.874226646144556,0.177969524989418,-0.451724052210951));
#8528=DIRECTION('',(0.578201042698217,-0.129292644584796,0.805584859762747));
#8529=DIRECTION('',(0.815249828314457,0.0523161665774051,-0.576741481209644));
#8530=DIRECTION('',(-0.568651450943455,0.253499412054562,-0.782543018260271));
#8531=DIRECTION('',(-0.775130086891539,0.153293179919426,0.612922955505588));
#8532=DIRECTION('',(0.947463063734865,0.256939463816866,-0.190514710171275));
#8533=DIRECTION('',(-0.15639107915377,-0.147454612865507,-0.976626319277646));
#8534=DIRECTION('',(0.461133313595748,0.638546144565041,-0.616128954321517));
#8535=DIRECTION('',(-0.120332780197176,0.732949598590468,0.669555754165469));
#8536=DIRECTION('',(0.274581936962134,0.831493960146459,0.482931210561176));
#8537=DIRECTION('',(-0.558407030198469,0.546756325920671,-0.623890301808463));
#8538=DIRECTION('',(-0.0970590015468771,0.464727477559394,-0.880118129468997));
#8539=DIRECTION('',(-0.10741718024211,0.874236680429436,0.47346781937166));
#8540=DIRECTION('',(0.788369383096707,0.585877248824415,0.187674092792938));
#8541=DIRECTION('',(-0.401734767447142,0.721312299802403,-0.564196546230087));
#8542=DIRECTION('',(0.715561648910992,0.371065766839458,-0.591846030051421));
#8543=DIRECTION('',(0.110146614204902,0.77671691745262,0.620143978058399));
#8544=DIRECTION('',(0.141178161620688,0.630384578185218,0.763337415739362));
#8545=DIRECTION('',(-0.631673159131479,0.651063559040613,-0.420838760242242));
#8546=DIRECTION('',(0.535942430847444,0.697767549108387,0.475274823895194));
#8547=DIRECTION('',(-0.762495380267419,0.158374864388854,0.627310287976099));
#8548=DIRECTION('',(-0.712490584419659,0.701207600870698,0.025788904484136));
#8549=DIRECTION('',(-0.175378172690868,-0.14237292839608,-0.974152167684052));
#8550=DIRECTION('',(-0.884399928949423,0.296232841948602,-0.360670027899894));
#8551=DIRECTION('',(-0.376865877917927,0.00261806662510259,0.926264139318962));
#8552=DIRECTION('',(0.735315553667162,0.145849108768166,-0.661845203961385));
#8553=DIRECTION('',(-0.617620808681115,-0.257854199875291,-0.743004541231586));
#8554=DIRECTION('axis',(0.,0.,1.));
#8555=DIRECTION('refdir',(1.,0.,0.));
#8556=DIRECTION('center_axis',(0.,-1.,0.));
#8557=DIRECTION('ref_axis',(0.,0.,-1.));
#8558=DIRECTION('center_axis',(0.,-1.,0.));
#8559=DIRECTION('ref_axis',(0.,0.,-1.));
#8560=DIRECTION('',(4.27395569285715E-18,0.999390827019096,-0.034899496702501));
#8561=DIRECTION('center_axis',(0.,-1.,0.));
#8562=DIRECTION('ref_axis',(0.,0.,-1.));
#8563=DIRECTION('center_axis',(0.,-1.,0.));
#8564=DIRECTION('ref_axis',(0.,0.,-1.));
#8565=DIRECTION('center_axis',(0.,-1.,0.));
#8566=DIRECTION('ref_axis',(0.,0.,-1.));
#8567=DIRECTION('center_axis',(0.,-1.,0.));
#8568=DIRECTION('ref_axis',(0.,0.,-1.));
#8569=DIRECTION('center_axis',(0.,-1.,0.));
#8570=DIRECTION('ref_axis',(0.,0.,-1.));
#8571=DIRECTION('center_axis',(0.,1.,0.));
#8572=DIRECTION('ref_axis',(0.,0.,1.));
#8573=DIRECTION('',(0.,-1.,0.));
#8574=DIRECTION('center_axis',(0.,-1.,0.));
#8575=DIRECTION('ref_axis',(0.,0.,-1.));
#8576=DIRECTION('center_axis',(0.,-1.,0.));
#8577=DIRECTION('ref_axis',(0.,0.,-1.));
#8578=DIRECTION('center_axis',(0.,-1.,0.));
#8579=DIRECTION('ref_axis',(0.,0.,-1.));
#8580=DIRECTION('center_axis',(0.,-1.,0.));
#8581=DIRECTION('ref_axis',(0.,0.,-1.));
#8582=DIRECTION('',(0.,-1.,0.));
#8583=DIRECTION('',(0.,0.,1.));
#8584=DIRECTION('',(1.,0.,0.));
#8585=DIRECTION('',(0.,0.,1.));
#8586=DIRECTION('',(1.,0.,0.));
#8587=DIRECTION('',(2.47697642240655E-17,-0.152596401142835,0.988288590624345));
#8588=DIRECTION('',(1.,2.99884974081348E-17,-2.0432925802721E-17));
#8589=DIRECTION('',(0.581607909236909,-0.162498735572193,-0.797073648322732));
#8590=DIRECTION('',(-0.80031129315564,0.0612196908231697,-0.596451157684402));
#8591=DIRECTION('',(0.546013883993754,0.,-0.837776126710505));
#8592=DIRECTION('',(-0.837776126710505,0.,-0.546013883993754));
#8593=CARTESIAN_POINT('',(0.,0.,0.));
#8594=CARTESIAN_POINT('',(0.,0.,0.));
#8595=CARTESIAN_POINT('Origin',(-99.7519848385422,5.,-11.9999999999999));
#8596=CARTESIAN_POINT('',(-125.680065601265,5.,25.0000000000001));
#8597=CARTESIAN_POINT('',(-65.6680057154831,5.,25.0000000000001));
#8598=CARTESIAN_POINT('',(-125.680324030103,5.,25.0000000000001));
#8599=CARTESIAN_POINT('',(-65.6680057154831,5.,-48.9999999999999));
#8600=CARTESIAN_POINT('',(-65.6680057154831,5.,25.0000000000001));
#8601=CARTESIAN_POINT('',(-125.680065601265,5.00000000000001,-48.9999999999999));
#8602=CARTESIAN_POINT('',(-125.680324030103,5.,-48.9999999999999));
#8603=CARTESIAN_POINT('',(-125.68006560189,4.99999999980206,-58.9999999999999));
#8604=CARTESIAN_POINT('',(-125.680065601265,5.,-48.9999999999999));
#8605=CARTESIAN_POINT('',(-145.859521458148,5.,-58.9999999999999));
#8606=CARTESIAN_POINT('',(-125.680065601745,5.,-58.9999999999999));
#8607=CARTESIAN_POINT('',(-145.859521458148,5.,35.0000000000001));
#8608=CARTESIAN_POINT('Origin',(-99.7519848385422,5.,-11.9999999999999));
#8609=CARTESIAN_POINT('',(-125.68006560126,5.00000000000148,35.0000000000001));
#8610=CARTESIAN_POINT('',(-145.859521458148,5.,35.0000000000001));
#8611=CARTESIAN_POINT('',(-125.680065601264,5.,25.0000000000001));
#8612=CARTESIAN_POINT('',(-88.9375988864104,5.,-15.9999999999999));
#8613=CARTESIAN_POINT('Origin',(-88.9375988864104,5.,-11.9999999999999));
#8614=CARTESIAN_POINT('',(-115.629992744845,5.,-27.9631510575948));
#8615=CARTESIAN_POINT('Origin',(-115.629992744845,5.,-11.9999999999999));
#8616=CARTESIAN_POINT('',(-142.322386603279,5.,-15.9999999999999));
#8617=CARTESIAN_POINT('Origin',(-142.322386603279,5.,-11.9999999999999));
#8618=CARTESIAN_POINT('Origin',(-145.859521458148,-5.,144.542028553823));
#8619=CARTESIAN_POINT('',(145.859521458148,-4.99999999999998,-59.));
#8620=CARTESIAN_POINT('',(36.8276756314269,-4.99999999999994,-157.982075177761));
#8621=CARTESIAN_POINT('Origin',(145.859521458148,-4.99999999999993,-168.542028553823));
#8622=CARTESIAN_POINT('',(145.859521458148,-5.,35.0000000000001));
#8623=CARTESIAN_POINT('Origin',(99.7519848385422,-5.,-11.9999999999999));
#8624=CARTESIAN_POINT('',(36.827675631427,-5.,133.982075177761));
#8625=CARTESIAN_POINT('Origin',(145.859521458148,-5.,144.542028553823));
#8626=CARTESIAN_POINT('',(-36.8276756314269,-5.,133.982075177761));
#8627=CARTESIAN_POINT('Origin',(0.,-5.,130.415240784856));
#8628=CARTESIAN_POINT('',(-145.859521458148,-5.,35.0000000000001));
#8629=CARTESIAN_POINT('Origin',(-145.859521458148,-5.,144.542028553823));
#8630=CARTESIAN_POINT('',(-145.859521458148,-4.99999999999998,-58.9999999999999));
#8631=CARTESIAN_POINT('Origin',(-99.7519848385422,-5.,-11.9999999999999));
#8632=CARTESIAN_POINT('',(-36.827675631427,-4.99999999999994,-157.982075177761));
#8633=CARTESIAN_POINT('Origin',(-145.859521458148,-4.99999999999993,-168.542028553823));
#8634=CARTESIAN_POINT('Origin',(-5.2737622621639E-14,-4.99999999999994,
-154.415240784856));
#8635=CARTESIAN_POINT('',(-20.,-5.,-48.9999999999999));
#8636=CARTESIAN_POINT('',(-20.,-5.,25.0000000000001));
#8637=CARTESIAN_POINT('',(-20.,-5.,-48.9999999999999));
#8638=CARTESIAN_POINT('',(-65.6680057154831,-5.,-48.9999999999999));
#8639=CARTESIAN_POINT('',(-65.6680057154831,-5.,-48.9999999999999));
#8640=CARTESIAN_POINT('',(-65.6680057154831,-5.,25.0000000000001));
#8641=CARTESIAN_POINT('',(-65.6680057154831,-5.,25.0000000000001));
#8642=CARTESIAN_POINT('',(-20.,-5.,25.0000000000001));
#8643=CARTESIAN_POINT('',(88.9375988864104,-5.,-15.9999999999999));
#8644=CARTESIAN_POINT('Origin',(88.9375988864104,-5.,-11.9999999999999));
#8645=CARTESIAN_POINT('',(115.629992744845,-5.,-27.9631510575948));
#8646=CARTESIAN_POINT('Origin',(115.629992744845,-5.,-11.9999999999999));
#8647=CARTESIAN_POINT('',(142.322386603279,-5.,-15.9999999999999));
#8648=CARTESIAN_POINT('Origin',(142.322386603279,-5.,-11.9999999999999));
#8649=CARTESIAN_POINT('',(-88.9375988864104,-5.,-15.9999999999999));
#8650=CARTESIAN_POINT('Origin',(-88.9375988864104,-5.,-11.9999999999999));
#8651=CARTESIAN_POINT('',(-115.629992744845,-5.,-27.9631510575948));
#8652=CARTESIAN_POINT('Origin',(-115.629992744845,-5.,-11.9999999999999));
#8653=CARTESIAN_POINT('',(-142.322386603279,-5.,-15.9999999999999));
#8654=CARTESIAN_POINT('Origin',(-142.322386603279,-5.,-11.9999999999999));
#8655=CARTESIAN_POINT('',(65.6680057154831,-5.,-48.9999999999999));
#8656=CARTESIAN_POINT('',(20.,-5.,-48.9999999999999));
#8657=CARTESIAN_POINT('',(65.6680057154831,-5.,-48.9999999999999));
#8658=CARTESIAN_POINT('',(20.,-5.,25.0000000000001));
#8659=CARTESIAN_POINT('',(20.,-5.,-48.9999999999999));
#8660=CARTESIAN_POINT('',(65.6680057154831,-5.,25.0000000000001));
#8661=CARTESIAN_POINT('',(20.,-5.,25.0000000000001));
#8662=CARTESIAN_POINT('',(65.6680057154831,-5.,25.0000000000001));
#8663=CARTESIAN_POINT('Origin',(0.,-5.00102500000001,-11.9999999999999));
#8664=CARTESIAN_POINT('',(0.,29.,-25.9999999999999));
#8665=CARTESIAN_POINT('Origin',(0.,29.,-11.9999999999999));
#8666=CARTESIAN_POINT('',(-1.71450551880629E-15,89.,-25.9999999999999));
#8667=CARTESIAN_POINT('',(-1.71450551880629E-15,-5.00102500000001,-25.9999999999999));
#8668=CARTESIAN_POINT('Origin',(0.,89.,-11.9999999999999));
#8669=CARTESIAN_POINT('',(-1.6909481438847,54.6122755947453,1.89750676829103));
#8670=CARTESIAN_POINT('',(-1.69094814388458,54.6122755947453,-25.8975067682909));
#8671=CARTESIAN_POINT('Ctrl Pts',(-1.69094814388471,54.6122755947453,1.89750676829103));
#8672=CARTESIAN_POINT('Ctrl Pts',(-1.69094814388471,54.9213889364491,1.89750676829103));
#8673=CARTESIAN_POINT('Ctrl Pts',(-1.76916191043536,55.1731377228307,1.88812065613091));
#8674=CARTESIAN_POINT('Ctrl Pts',(-1.9656264409252,55.6361599846496,1.86167854986234));
#8675=CARTESIAN_POINT('Ctrl Pts',(-2.08733509638717,55.8459330182592,1.84417693298648));
#8676=CARTESIAN_POINT('Ctrl Pts',(-2.48603840542449,56.4613583117431,1.78012768145208));
#8677=CARTESIAN_POINT('Ctrl Pts',(-2.79295687688375,56.8454209830934,1.72280566002277));
#8678=CARTESIAN_POINT('Ctrl Pts',(-3.78895528995958,58.0297922078367,1.49473345638479));
#8679=CARTESIAN_POINT('Ctrl Pts',(-4.53827705470844,58.8319051311986,1.27093230580055));
#8680=CARTESIAN_POINT('Ctrl Pts',(-6.10105549036539,60.4801717461623,0.628963504710961));
#8681=CARTESIAN_POINT('Ctrl Pts',(-6.91295780738778,61.3175968721307,0.21097588427962));
#8682=CARTESIAN_POINT('Ctrl Pts',(-8.49452237285656,62.9386948354568,-0.831293369425304));
#8683=CARTESIAN_POINT('Ctrl Pts',(-9.26451807446147,63.7219839395944,-1.45566578996009));
#8684=CARTESIAN_POINT('Ctrl Pts',(-11.0655427499361,65.5494769648951,-3.28315881526074));
#8685=CARTESIAN_POINT('Ctrl Pts',(-12.116208359012,66.610305038754,-4.74556937837982));
#8686=CARTESIAN_POINT('Ctrl Pts',(-13.2182983629377,67.7220613929565,-7.29533046872904));
#8687=CARTESIAN_POINT('Ctrl Pts',(-13.5094758463079,68.0155297755796,-8.20393179374744));
#8688=CARTESIAN_POINT('Ctrl Pts',(-13.90040638973,68.4094703383725,-10.0778205894963));
#8689=CARTESIAN_POINT('Ctrl Pts',(-14.,68.5097823630363,-11.043174986104));
#8690=CARTESIAN_POINT('Ctrl Pts',(-14.,68.5097823630363,-12.9568250138958));
#8691=CARTESIAN_POINT('Ctrl Pts',(-13.90040638973,68.4094703383725,-13.9221794105036));
#8692=CARTESIAN_POINT('Ctrl Pts',(-13.5094758463079,68.0155297755796,-15.7960682062524));
#8693=CARTESIAN_POINT('Ctrl Pts',(-13.2182983629377,67.7220613929565,-16.7046695312708));
#8694=CARTESIAN_POINT('Ctrl Pts',(-12.116208359012,66.610305038754,-19.25443062162));
#8695=CARTESIAN_POINT('Ctrl Pts',(-11.0655427499361,65.5494769648951,-20.7168411847391));
#8696=CARTESIAN_POINT('Ctrl Pts',(-9.26451807446147,63.7219839395945,-22.5443342100398));
#8697=CARTESIAN_POINT('Ctrl Pts',(-8.49452237285657,62.9386948354569,-23.1687066305745));
#8698=CARTESIAN_POINT('Ctrl Pts',(-6.91295780738777,61.3175968721307,-24.2109758842795));
#8699=CARTESIAN_POINT('Ctrl Pts',(-6.10105549036536,60.4801717461623,-24.6289635047108));
#8700=CARTESIAN_POINT('Ctrl Pts',(-4.53827705470839,58.8319051311986,-25.2709323058004));
#8701=CARTESIAN_POINT('Ctrl Pts',(-3.78895528995955,58.0297922078367,-25.4947334563846));
#8702=CARTESIAN_POINT('Ctrl Pts',(-2.7929568768837,56.8454209830934,-25.7228056600226));
#8703=CARTESIAN_POINT('Ctrl Pts',(-2.48603840542445,56.4613583117431,-25.7801276814519));
#8704=CARTESIAN_POINT('Ctrl Pts',(-2.0873350963871,55.8459330182592,-25.8441769329863));
#8705=CARTESIAN_POINT('Ctrl Pts',(-1.9656264409251,55.6361599846497,-25.8616785498622));
#8706=CARTESIAN_POINT('Ctrl Pts',(-1.76916191043525,55.1731377228307,-25.8881206561308));
#8707=CARTESIAN_POINT('Ctrl Pts',(-1.69094814388459,54.9213889364491,-25.8975067682909));
#8708=CARTESIAN_POINT('Ctrl Pts',(-1.69094814388459,54.6122755947453,-25.8975067682909));
#8709=CARTESIAN_POINT('Ctrl Pts',(-1.69094814388459,54.6122755947453,-25.8975067682909));
#8710=CARTESIAN_POINT('Ctrl Pts',(-1.69094814388459,54.3031622530416,-25.8975067682909));
#8711=CARTESIAN_POINT('Ctrl Pts',(-1.76916191043526,54.05141346666,-25.8881206561308));
#8712=CARTESIAN_POINT('Ctrl Pts',(-1.96562644092511,53.588391204841,-25.8616785498622));
#8713=CARTESIAN_POINT('Ctrl Pts',(-2.08733509638708,53.3786181712314,-25.8441769329863));
#8714=CARTESIAN_POINT('Ctrl Pts',(-2.48603840542441,52.7631928777475,-25.7801276814519));
#8715=CARTESIAN_POINT('Ctrl Pts',(-2.79295687688368,52.3791302063973,-25.7228056600226));
#8716=CARTESIAN_POINT('Ctrl Pts',(-3.78895528995951,51.194758981654,-25.4947334563847));
#8717=CARTESIAN_POINT('Ctrl Pts',(-4.53827705470836,50.3926460582921,-25.2709323058004));
#8718=CARTESIAN_POINT('Ctrl Pts',(-6.10105549036533,48.7443794433284,-24.6289635047108));
#8719=CARTESIAN_POINT('Ctrl Pts',(-6.91295780738773,47.90695431736,-24.2109758842795));
#8720=CARTESIAN_POINT('Ctrl Pts',(-8.49452237285654,46.2858563540338,-23.1687066305746));
#8721=CARTESIAN_POINT('Ctrl Pts',(-9.26451807446145,45.5025672498962,-22.5443342100398));
#8722=CARTESIAN_POINT('Ctrl Pts',(-11.0655427499361,43.6750742245956,-20.7168411847391));
#8723=CARTESIAN_POINT('Ctrl Pts',(-12.116208359012,42.6142461507366,-19.25443062162));
#8724=CARTESIAN_POINT('Ctrl Pts',(-13.2182983629377,41.5024897965342,-16.7046695312708));
#8725=CARTESIAN_POINT('Ctrl Pts',(-13.5094758463079,41.2090214139111,-15.7960682062524));
#8726=CARTESIAN_POINT('Ctrl Pts',(-13.90040638973,40.8150808511182,-13.9221794105036));
#8727=CARTESIAN_POINT('Ctrl Pts',(-14.,40.7147688264544,-12.9568250138958));
#8728=CARTESIAN_POINT('Ctrl Pts',(-14.,40.7147688264544,-11.043174986104));
#8729=CARTESIAN_POINT('Ctrl Pts',(-13.90040638973,40.8150808511182,-10.0778205894962));
#8730=CARTESIAN_POINT('Ctrl Pts',(-13.5094758463079,41.2090214139111,-8.20393179374744));
#8731=CARTESIAN_POINT('Ctrl Pts',(-13.2182983629377,41.5024897965342,-7.29533046872903));
#8732=CARTESIAN_POINT('Ctrl Pts',(-12.116208359012,42.6142461507366,-4.74556937837981));
#8733=CARTESIAN_POINT('Ctrl Pts',(-11.0655427499361,43.6750742245956,-3.28315881526073));
#8734=CARTESIAN_POINT('Ctrl Pts',(-9.26451807446146,45.5025672498962,-1.45566578996008));
#8735=CARTESIAN_POINT('Ctrl Pts',(-8.49452237285655,46.2858563540338,-0.831293369425292));
#8736=CARTESIAN_POINT('Ctrl Pts',(-6.91295780738776,47.90695431736,0.210975884279631));
#8737=CARTESIAN_POINT('Ctrl Pts',(-6.10105549036537,48.7443794433284,0.628963504710973));
#8738=CARTESIAN_POINT('Ctrl Pts',(-4.53827705470841,50.3926460582921,1.27093230580056));
#8739=CARTESIAN_POINT('Ctrl Pts',(-3.78895528995956,51.194758981654,1.4947334563848));
#8740=CARTESIAN_POINT('Ctrl Pts',(-2.79295687688373,52.3791302063973,1.72280566002277));
#8741=CARTESIAN_POINT('Ctrl Pts',(-2.48603840542447,52.7631928777476,1.78012768145208));
#8742=CARTESIAN_POINT('Ctrl Pts',(-2.08733509638715,53.3786181712315,1.84417693298648));
#8743=CARTESIAN_POINT('Ctrl Pts',(-1.96562644092519,53.588391204841,1.86167854986234));
#8744=CARTESIAN_POINT('Ctrl Pts',(-1.76916191043536,54.05141346666,1.88812065613091));
#8745=CARTESIAN_POINT('Ctrl Pts',(-1.6909481438847,54.3031622530416,1.89750676829103));
#8746=CARTESIAN_POINT('Ctrl Pts',(-1.69094814388471,54.6122755947453,1.89750676829103));
#8747=CARTESIAN_POINT('',(1.69094814388473,54.6122755947453,1.89750676829103));
#8748=CARTESIAN_POINT('',(1.69094814388458,54.6122755947453,-25.8975067682909));
#8749=CARTESIAN_POINT('Ctrl Pts',(1.69094814388471,54.6122755947453,1.89750676829103));
#8750=CARTESIAN_POINT('Ctrl Pts',(1.6909481438847,54.3031622530416,1.89750676829103));
#8751=CARTESIAN_POINT('Ctrl Pts',(1.76916191043536,54.05141346666,1.88812065613091));
#8752=CARTESIAN_POINT('Ctrl Pts',(1.96562644092519,53.588391204841,1.86167854986234));
#8753=CARTESIAN_POINT('Ctrl Pts',(2.08733509638715,53.3786181712315,1.84417693298648));
#8754=CARTESIAN_POINT('Ctrl Pts',(2.48603840542448,52.7631928777475,1.78012768145208));
#8755=CARTESIAN_POINT('Ctrl Pts',(2.79295687688374,52.3791302063973,1.72280566002277));
#8756=CARTESIAN_POINT('Ctrl Pts',(3.78895528995957,51.194758981654,1.49473345638479));
#8757=CARTESIAN_POINT('Ctrl Pts',(4.53827705470842,50.3926460582921,1.27093230580055));
#8758=CARTESIAN_POINT('Ctrl Pts',(6.10105549036537,48.7443794433283,0.62896350471097));
#8759=CARTESIAN_POINT('Ctrl Pts',(6.91295780738778,47.90695431736,0.210975884279621));
#8760=CARTESIAN_POINT('Ctrl Pts',(8.49452237285656,46.2858563540338,-0.831293369425302));
#8761=CARTESIAN_POINT('Ctrl Pts',(9.26451807446146,45.5025672498962,-1.45566578996008));
#8762=CARTESIAN_POINT('Ctrl Pts',(11.0655427499361,43.6750742245956,-3.28315881526073));
#8763=CARTESIAN_POINT('Ctrl Pts',(12.116208359012,42.6142461507366,-4.74556937837981));
#8764=CARTESIAN_POINT('Ctrl Pts',(13.2182983629377,41.5024897965342,-7.29533046872903));
#8765=CARTESIAN_POINT('Ctrl Pts',(13.5094758463079,41.2090214139111,-8.20393179374743));
#8766=CARTESIAN_POINT('Ctrl Pts',(13.90040638973,40.8150808511182,-10.0778205894962));
#8767=CARTESIAN_POINT('Ctrl Pts',(14.,40.7147688264544,-11.043174986104));
#8768=CARTESIAN_POINT('Ctrl Pts',(14.,40.7147688264544,-12.9568250138958));
#8769=CARTESIAN_POINT('Ctrl Pts',(13.90040638973,40.8150808511182,-13.9221794105036));
#8770=CARTESIAN_POINT('Ctrl Pts',(13.5094758463079,41.2090214139111,-15.7960682062524));
#8771=CARTESIAN_POINT('Ctrl Pts',(13.2182983629377,41.5024897965342,-16.7046695312708));
#8772=CARTESIAN_POINT('Ctrl Pts',(12.116208359012,42.6142461507366,-19.25443062162));
#8773=CARTESIAN_POINT('Ctrl Pts',(11.0655427499361,43.6750742245956,-20.7168411847391));
#8774=CARTESIAN_POINT('Ctrl Pts',(9.26451807446145,45.5025672498962,-22.5443342100398));
#8775=CARTESIAN_POINT('Ctrl Pts',(8.49452237285654,46.2858563540338,-23.1687066305745));
#8776=CARTESIAN_POINT('Ctrl Pts',(6.91295780738774,47.90695431736,-24.2109758842795));
#8777=CARTESIAN_POINT('Ctrl Pts',(6.10105549036533,48.7443794433284,-24.6289635047108));
#8778=CARTESIAN_POINT('Ctrl Pts',(4.53827705470836,50.3926460582921,-25.2709323058004));
#8779=CARTESIAN_POINT('Ctrl Pts',(3.78895528995951,51.194758981654,-25.4947334563847));
#8780=CARTESIAN_POINT('Ctrl Pts',(2.79295687688367,52.3791302063973,-25.7228056600226));
#8781=CARTESIAN_POINT('Ctrl Pts',(2.48603840542441,52.7631928777475,-25.7801276814519));
#8782=CARTESIAN_POINT('Ctrl Pts',(2.08733509638707,53.3786181712314,-25.8441769329863));
#8783=CARTESIAN_POINT('Ctrl Pts',(1.9656264409251,53.588391204841,-25.8616785498622));
#8784=CARTESIAN_POINT('Ctrl Pts',(1.76916191043527,54.05141346666,-25.8881206561308));
#8785=CARTESIAN_POINT('Ctrl Pts',(1.69094814388459,54.3031622530415,-25.8975067682909));
#8786=CARTESIAN_POINT('Ctrl Pts',(1.69094814388459,54.6122755947453,-25.8975067682909));
#8787=CARTESIAN_POINT('Ctrl Pts',(1.69094814388459,54.6122755947453,-25.8975067682909));
#8788=CARTESIAN_POINT('Ctrl Pts',(1.69094814388459,54.9213889364491,-25.8975067682909));
#8789=CARTESIAN_POINT('Ctrl Pts',(1.76916191043525,55.1731377228307,-25.8881206561308));
#8790=CARTESIAN_POINT('Ctrl Pts',(1.9656264409251,55.6361599846497,-25.8616785498622));
#8791=CARTESIAN_POINT('Ctrl Pts',(2.0873350963871,55.8459330182592,-25.8441769329863));
#8792=CARTESIAN_POINT('Ctrl Pts',(2.48603840542444,56.4613583117431,-25.7801276814519));
#8793=CARTESIAN_POINT('Ctrl Pts',(2.79295687688369,56.8454209830934,-25.7228056600226));
#8794=CARTESIAN_POINT('Ctrl Pts',(3.78895528995954,58.0297922078367,-25.4947334563846));
#8795=CARTESIAN_POINT('Ctrl Pts',(4.53827705470839,58.8319051311986,-25.2709323058004));
#8796=CARTESIAN_POINT('Ctrl Pts',(6.10105549036536,60.4801717461623,-24.6289635047108));
#8797=CARTESIAN_POINT('Ctrl Pts',(6.91295780738777,61.3175968721307,-24.2109758842795));
#8798=CARTESIAN_POINT('Ctrl Pts',(8.49452237285657,62.9386948354569,-23.1687066305745));
#8799=CARTESIAN_POINT('Ctrl Pts',(9.26451807446147,63.7219839395945,-22.5443342100398));
#8800=CARTESIAN_POINT('Ctrl Pts',(11.0655427499361,65.5494769648951,-20.7168411847391));
#8801=CARTESIAN_POINT('Ctrl Pts',(12.116208359012,66.610305038754,-19.25443062162));
#8802=CARTESIAN_POINT('Ctrl Pts',(13.2182983629377,67.7220613929565,-16.7046695312708));
#8803=CARTESIAN_POINT('Ctrl Pts',(13.5094758463079,68.0155297755796,-15.7960682062524));
#8804=CARTESIAN_POINT('Ctrl Pts',(13.90040638973,68.4094703383725,-13.9221794105036));
#8805=CARTESIAN_POINT('Ctrl Pts',(14.,68.5097823630363,-12.9568250138958));
#8806=CARTESIAN_POINT('Ctrl Pts',(14.,68.5097823630363,-11.0431749861041));
#8807=CARTESIAN_POINT('Ctrl Pts',(13.90040638973,68.4094703383725,-10.0778205894963));
#8808=CARTESIAN_POINT('Ctrl Pts',(13.5094758463079,68.0155297755796,-8.20393179374744));
#8809=CARTESIAN_POINT('Ctrl Pts',(13.2182983629377,67.7220613929565,-7.29533046872904));
#8810=CARTESIAN_POINT('Ctrl Pts',(12.116208359012,66.610305038754,-4.74556937837982));
#8811=CARTESIAN_POINT('Ctrl Pts',(11.0655427499361,65.5494769648951,-3.28315881526074));
#8812=CARTESIAN_POINT('Ctrl Pts',(9.26451807446147,63.7219839395944,-1.45566578996009));
#8813=CARTESIAN_POINT('Ctrl Pts',(8.49452237285658,62.9386948354569,-0.831293369425317));
#8814=CARTESIAN_POINT('Ctrl Pts',(6.91295780738779,61.3175968721307,0.210975884279613));
#8815=CARTESIAN_POINT('Ctrl Pts',(6.10105549036539,60.4801717461623,0.628963504710959));
#8816=CARTESIAN_POINT('Ctrl Pts',(4.53827705470844,58.8319051311986,1.27093230580055));
#8817=CARTESIAN_POINT('Ctrl Pts',(3.78895528995959,58.0297922078367,1.49473345638479));
#8818=CARTESIAN_POINT('Ctrl Pts',(2.79295687688376,56.8454209830934,1.72280566002277));
#8819=CARTESIAN_POINT('Ctrl Pts',(2.4860384054245,56.4613583117431,1.78012768145208));
#8820=CARTESIAN_POINT('Ctrl Pts',(2.08733509638718,55.8459330182592,1.84417693298648));
#8821=CARTESIAN_POINT('Ctrl Pts',(1.96562644092521,55.6361599846497,1.86167854986234));
#8822=CARTESIAN_POINT('Ctrl Pts',(1.76916191043537,55.1731377228307,1.88812065613091));
#8823=CARTESIAN_POINT('Ctrl Pts',(1.6909481438847,54.9213889364491,1.89750676829103));
#8824=CARTESIAN_POINT('Ctrl Pts',(1.6909481438847,54.6122755947453,1.89750676829103));
#8825=CARTESIAN_POINT('Origin',(165.591979774207,54.6122755947453,-12.));
#8826=CARTESIAN_POINT('',(45.,54.6122755947453,-25.8975067682909));
#8827=CARTESIAN_POINT('Origin',(45.,54.6122755947453,-11.9999999999999));
#8828=CARTESIAN_POINT('',(165.591979774207,54.6122755947453,-25.8975067682909));
#8829=CARTESIAN_POINT('Origin',(5.94655548926424E-16,26.2427388041954,25.0000000000001));
#8830=CARTESIAN_POINT('',(-20.,72.1122755947453,-48.9999999999999));
#8831=CARTESIAN_POINT('',(-20.,72.1122755947453,-11.9999999999999));
#8832=CARTESIAN_POINT('',(-20.,72.1122755947453,-48.9999999999999));
#8833=CARTESIAN_POINT('',(-1.14423774522196E-16,76.2828667554667,-31.9999999999999));
#8834=CARTESIAN_POINT('Ctrl Pts',(1.38777878078145E-15,76.2828667554667,
-31.9999999999999));
#8835=CARTESIAN_POINT('Ctrl Pts',(-1.2705472609979,76.2828667554667,-31.9999999999999));
#8836=CARTESIAN_POINT('Ctrl Pts',(-2.58007773937013,76.2332652071209,-31.8769708923002));
#8837=CARTESIAN_POINT('Ctrl Pts',(-5.17618585589728,76.0314587231336,-31.3638289853873));
#8838=CARTESIAN_POINT('Ctrl Pts',(-6.46280366693617,75.8793792723685,-30.9738701002276));
#8839=CARTESIAN_POINT('Ctrl Pts',(-8.92278917996998,75.4966497262723,-29.9487995317102));
#8840=CARTESIAN_POINT('Ctrl Pts',(-10.0983665793023,75.2659618277825,-29.3128730480594));
#8841=CARTESIAN_POINT('Ctrl Pts',(-12.2682645673177,74.7684339328333,-27.8493616648039));
#8842=CARTESIAN_POINT('Ctrl Pts',(-13.2626071807075,74.5020216025358,-27.0216640667543));
#8843=CARTESIAN_POINT('Ctrl Pts',(-15.0225516277294,73.9834946181185,-25.2617196197324));
#8844=CARTESIAN_POINT('Ctrl Pts',(-15.8503625531969,73.7125357294074,-24.2669504874496));
#8845=CARTESIAN_POINT('Ctrl Pts',(-17.3134969066183,73.1986589652098,-22.0972715139887));
#8846=CARTESIAN_POINT('Ctrl Pts',(-17.9489707104667,72.9562551485406,-20.9223413606241));
#8847=CARTESIAN_POINT('Ctrl Pts',(-18.9735260730669,72.5495796554118,-18.4636662849712));
#8848=CARTESIAN_POINT('Ctrl Pts',(-19.363419845374,72.3854545732174,-17.1776933689394));
#8849=CARTESIAN_POINT('Ctrl Pts',(-19.876740954423,72.1666695578122,-14.5818027748883));
#8850=CARTESIAN_POINT('Ctrl Pts',(-20.,72.1122755947453,-13.2718294118763));
#8851=CARTESIAN_POINT('Ctrl Pts',(-20.,72.1122755947453,-11.9999999999999));
#8852=CARTESIAN_POINT('',(20.,72.1122755947453,-11.9999999999999));
#8853=CARTESIAN_POINT('Ctrl Pts',(20.,72.1122755947453,-11.9999999999999));
#8854=CARTESIAN_POINT('Ctrl Pts',(20.,72.1122755947453,-13.2718294118763));
#8855=CARTESIAN_POINT('Ctrl Pts',(19.876740954423,72.1666695578122,-14.5818027748883));
#8856=CARTESIAN_POINT('Ctrl Pts',(19.363419845374,72.3854545732174,-17.1776933689394));
#8857=CARTESIAN_POINT('Ctrl Pts',(18.9735260730669,72.5495796554118,-18.4636662849712));
#8858=CARTESIAN_POINT('Ctrl Pts',(17.9489707104667,72.9562551485406,-20.922341360624));
#8859=CARTESIAN_POINT('Ctrl Pts',(17.3134969066183,73.1986589652098,-22.0972715139887));
#8860=CARTESIAN_POINT('Ctrl Pts',(15.8503625531969,73.7125357294074,-24.2669504874496));
#8861=CARTESIAN_POINT('Ctrl Pts',(15.0225516277294,73.9834946181185,-25.2617196197324));
#8862=CARTESIAN_POINT('Ctrl Pts',(13.2626071807075,74.5020216025358,-27.0216640667543));
#8863=CARTESIAN_POINT('Ctrl Pts',(12.2682645673177,74.7684339328333,-27.8493616648039));
#8864=CARTESIAN_POINT('Ctrl Pts',(10.0983665793023,75.2659618277825,-29.3128730480594));
#8865=CARTESIAN_POINT('Ctrl Pts',(8.92278917996999,75.4966497262723,-29.9487995317102));
#8866=CARTESIAN_POINT('Ctrl Pts',(6.46280366693618,75.8793792723685,-30.9738701002276));
#8867=CARTESIAN_POINT('Ctrl Pts',(5.17618585589729,76.0314587231336,-31.3638289853873));
#8868=CARTESIAN_POINT('Ctrl Pts',(2.58007773937014,76.2332652071209,-31.8769708923002));
#8869=CARTESIAN_POINT('Ctrl Pts',(1.2705472609979,76.2828667554667,-31.9999999999999));
#8870=CARTESIAN_POINT('Ctrl Pts',(1.66533453693773E-15,76.2828667554667,
-31.9999999999999));
#8871=CARTESIAN_POINT('',(20.,72.1122755947453,-48.9999999999999));
#8872=CARTESIAN_POINT('',(20.,72.1122755947453,-48.9999999999999));
#8873=CARTESIAN_POINT('',(37.,59.9327136539873,-48.9999999999999));
#8874=CARTESIAN_POINT('Origin',(-1.31067715332243E-14,26.2427388041954,
-48.9999999999999));
#8875=CARTESIAN_POINT('',(37.,59.9327136539873,-58.9999999999999));
#8876=CARTESIAN_POINT('',(37.,59.9327136539873,-48.9999999999999));
#8877=CARTESIAN_POINT('',(-37.,59.9327136539873,-58.9999999999999));
#8878=CARTESIAN_POINT('Ctrl Pts',(-37.,59.9327136539873,-58.9999999999999));
#8879=CARTESIAN_POINT('Ctrl Pts',(-34.9241175691101,62.2125506169229,-58.9999999999999));
#8880=CARTESIAN_POINT('Ctrl Pts',(-32.5494800245177,64.3947066833499,-58.9999999999999));
#8881=CARTESIAN_POINT('Ctrl Pts',(-29.8860954400449,66.3779565652608,-58.9999999999999));
#8882=CARTESIAN_POINT('Ctrl Pts',(-27.222710855572,68.3612064471717,-58.9999999999999));
#8883=CARTESIAN_POINT('Ctrl Pts',(-24.2700583438171,70.1440603895185,-58.9999999999999));
#8884=CARTESIAN_POINT('Ctrl Pts',(-21.0832893198028,71.6245558330132,-58.9999999999999));
#8885=CARTESIAN_POINT('Ctrl Pts',(-17.8965202957886,73.105051276508,-58.9999999999999));
#8886=CARTESIAN_POINT('Ctrl Pts',(-14.4761422078645,74.2813950126213,-58.9999999999999));
#8887=CARTESIAN_POINT('Ctrl Pts',(-10.9229576299852,75.0761638529584,-58.9999999999999));
#8888=CARTESIAN_POINT('Ctrl Pts',(-7.36977305210587,75.8709326932955,-58.9999999999999));
#8889=CARTESIAN_POINT('Ctrl Pts',(-3.68542231180591,76.2828667554667,-58.9999999999999));
#8890=CARTESIAN_POINT('Ctrl Pts',(-8.60422844084496E-15,76.2828667554667,
-58.9999999999999));
#8891=CARTESIAN_POINT('Ctrl Pts',(3.68542231180589,76.2828667554668,-58.9999999999999));
#8892=CARTESIAN_POINT('Ctrl Pts',(7.36977305210586,75.8709326932955,-58.9999999999999));
#8893=CARTESIAN_POINT('Ctrl Pts',(10.9229576299852,75.0761638529584,-58.9999999999999));
#8894=CARTESIAN_POINT('Ctrl Pts',(14.4761422078645,74.2813950126214,-58.9999999999999));
#8895=CARTESIAN_POINT('Ctrl Pts',(17.8965202957886,73.105051276508,-58.9999999999999));
#8896=CARTESIAN_POINT('Ctrl Pts',(21.0832893198028,71.6245558330132,-58.9999999999999));
#8897=CARTESIAN_POINT('Ctrl Pts',(24.270058343817,70.1440603895185,-58.9999999999999));
#8898=CARTESIAN_POINT('Ctrl Pts',(27.222710855572,68.3612064471716,-58.9999999999999));
#8899=CARTESIAN_POINT('Ctrl Pts',(29.8860954400449,66.3779565652607,-58.9999999999999));
#8900=CARTESIAN_POINT('Ctrl Pts',(32.5494800245177,64.3947066833499,-58.9999999999999));
#8901=CARTESIAN_POINT('Ctrl Pts',(34.9241175691101,62.2125506169228,-58.9999999999999));
#8902=CARTESIAN_POINT('Ctrl Pts',(37.,59.9327136539873,-58.9999999999999));
#8903=CARTESIAN_POINT('',(-37.,59.9327136539873,-48.9999999999999));
#8904=CARTESIAN_POINT('',(-37.,59.9327136539873,-48.9999999999999));
#8905=CARTESIAN_POINT('Origin',(-1.31067715332243E-14,26.2427388041954,
-48.9999999999999));
#8906=CARTESIAN_POINT('Origin',(-99.7519848385422,5.,-11.9999999999999));
#8907=CARTESIAN_POINT('',(65.6680057154831,5.,25.0000000000001));
#8908=CARTESIAN_POINT('',(65.6680057154831,5.,-48.9999999999999));
#8909=CARTESIAN_POINT('',(65.6680057154831,5.,25.0000000000001));
#8910=CARTESIAN_POINT('',(125.680065601264,4.99999999999998,25.0000000000001));
#8911=CARTESIAN_POINT('',(65.6680057154831,5.,25.0000000000001));
#8912=CARTESIAN_POINT('',(125.680065601264,5.,35.0000000000001));
#8913=CARTESIAN_POINT('',(125.680065601264,5.,25.0000000000001));
#8914=CARTESIAN_POINT('',(145.859521458148,5.,35.0000000000001));
#8915=CARTESIAN_POINT('',(125.680065601264,5.,35.0000000000001));
#8916=CARTESIAN_POINT('',(145.859521458148,5.,-59.));
#8917=CARTESIAN_POINT('Origin',(99.7519848385422,5.,-11.9999999999999));
#8918=CARTESIAN_POINT('',(125.68006560189,4.99999999980207,-59.));
#8919=CARTESIAN_POINT('',(145.859521458148,5.,-58.9999999999999));
#8920=CARTESIAN_POINT('',(125.680065601265,4.99999999999999,-49.));
#8921=CARTESIAN_POINT('',(125.680065601265,5.,-49.));
#8922=CARTESIAN_POINT('',(65.6680057154831,5.,-48.9999999999999));
#8923=CARTESIAN_POINT('',(88.9375988864104,5.,-15.9999999999999));
#8924=CARTESIAN_POINT('Origin',(88.9375988864104,5.,-11.9999999999999));
#8925=CARTESIAN_POINT('',(115.629992744845,5.,-27.9631510575948));
#8926=CARTESIAN_POINT('Origin',(115.629992744845,5.,-11.9999999999999));
#8927=CARTESIAN_POINT('',(142.322386603279,5.,-15.9999999999999));
#8928=CARTESIAN_POINT('Origin',(142.322386603279,5.,-11.9999999999999));
#8929=CARTESIAN_POINT('Origin',(-85.4296283056384,23.8067054410607,25.0000000000001));
#8930=CARTESIAN_POINT('',(-37.,59.9327136539873,25.0000000000001));
#8931=CARTESIAN_POINT('',(-20.,72.1122755947453,25.0000000000001));
#8932=CARTESIAN_POINT('Origin',(5.94655548926424E-16,26.2427388041954,25.0000000000001));
#8933=CARTESIAN_POINT('',(-20.,-5.,25.0000000000001));
#8934=CARTESIAN_POINT('',(-65.6680057154831,-5.,25.0000000000001));
#8935=CARTESIAN_POINT('Ctrl Pts',(-125.680065601265,4.99999999999999,25.0000000000001));
#8936=CARTESIAN_POINT('Ctrl Pts',(-124.960945054864,5.22751276297754,25.0000000000001));
#8937=CARTESIAN_POINT('Ctrl Pts',(-124.243155867433,5.46012087178501,25.0000000000001));
#8938=CARTESIAN_POINT('Ctrl Pts',(-123.527427567709,5.69757964881347,25.0000000000001));
#8939=CARTESIAN_POINT('Ctrl Pts',(-122.804827886392,5.93731815946461,25.0000000000001));
#8940=CARTESIAN_POINT('Ctrl Pts',(-122.084328820779,6.18200089120545,25.0000000000001));
#8941=CARTESIAN_POINT('Ctrl Pts',(-121.366643614241,6.43133795177422,25.0000000000001));
#8942=CARTESIAN_POINT('Ctrl Pts',(-120.640583813992,6.68358450045882,25.0000000000001));
#8943=CARTESIAN_POINT('Ctrl Pts',(-119.91740388334,6.94059459252451,25.0000000000001));
#8944=CARTESIAN_POINT('Ctrl Pts',(-119.19780468018,7.20202979663394,25.0000000000001));
#8945=CARTESIAN_POINT('Ctrl Pts',(-118.46820637769,7.46709774041672,25.0000000000001));
#8946=CARTESIAN_POINT('Ctrl Pts',(-117.742288953963,7.73671457758463,25.0000000000001));
#8947=CARTESIAN_POINT('Ctrl Pts',(-117.020745101533,8.01048912839484,25.0000000000001));
#8948=CARTESIAN_POINT('Ctrl Pts',(-116.287407035734,8.28873874396535,25.0000000000001));
#8949=CARTESIAN_POINT('Ctrl Pts',(-115.558586627373,8.57128304592011,25.0000000000001));
#8950=CARTESIAN_POINT('Ctrl Pts',(-114.834973164448,8.85767273946868,25.0000000000001));
#8951=CARTESIAN_POINT('Ctrl Pts',(-114.357879489923,9.0464955271055,25.0000000000001));
#8952=CARTESIAN_POINT('Ctrl Pts',(-113.883048517548,9.23698912926061,25.0000000000001));
#8953=CARTESIAN_POINT('Ctrl Pts',(-113.410669261531,9.42901606958512,25.0000000000001));
#8954=CARTESIAN_POINT('Ctrl Pts',(-113.363716076149,9.44810301384167,25.0000000000001));
#8955=CARTESIAN_POINT('Ctrl Pts',(-113.316778572265,9.46720857102223,25.0000000000001));
#8956=CARTESIAN_POINT('Ctrl Pts',(-113.269855341093,9.48633327990069,25.0000000000001));
#8957=CARTESIAN_POINT('Ctrl Pts',(-112.214947248068,9.91628683741896,25.0000000000001));
#8958=CARTESIAN_POINT('Ctrl Pts',(-111.167493669256,10.3558266948226,25.0000000000001));
#8959=CARTESIAN_POINT('Ctrl Pts',(-110.127707792712,10.804452542433,25.0000000000001));
#8960=CARTESIAN_POINT('Ctrl Pts',(-109.064746553832,11.2630776281616,25.0000000000001));
#8961=CARTESIAN_POINT('Ctrl Pts',(-108.00979854462,11.7311981609204,25.0000000000001));
#8962=CARTESIAN_POINT('Ctrl Pts',(-106.963052490346,12.2082398956616,25.0000000000001));
#8963=CARTESIAN_POINT('Ctrl Pts',(-105.889281591192,12.6975978735168,25.0000000000001));
#8964=CARTESIAN_POINT('Ctrl Pts',(-104.824141527827,13.1963435545408,25.0000000000001));
#8965=CARTESIAN_POINT('Ctrl Pts',(-103.76779680625,13.7038170919497,25.0000000000001));
#8966=CARTESIAN_POINT('Ctrl Pts',(-102.679455390731,14.2266620087278,25.0000000000001));
#8967=CARTESIAN_POINT('Ctrl Pts',(-101.600450087039,14.7587714042181,25.0000000000001));
#8968=CARTESIAN_POINT('Ctrl Pts',(-100.530921385051,15.2993833950381,25.0000000000001));
#8969=CARTESIAN_POINT('Ctrl Pts',(-100.159757279432,15.4869947846971,25.0000000000001));
#8970=CARTESIAN_POINT('Ctrl Pts',(-99.7897341428704,15.6756298332555,25.0000000000001));
#8971=CARTESIAN_POINT('Ctrl Pts',(-99.4208568320684,15.8652556601936,25.0000000000001));
#8972=CARTESIAN_POINT('Ctrl Pts',(-99.2980442797775,15.928388932706,25.0000000000001));
#8973=CARTESIAN_POINT('Ctrl Pts',(-99.1753587340892,15.9916320252805,25.0000000000001));
#8974=CARTESIAN_POINT('Ctrl Pts',(-99.0528003622234,16.054983712168,25.0000000000001));
#8975=CARTESIAN_POINT('Ctrl Pts',(-98.9807005502699,16.0922528488413,25.0000000000001));
#8976=CARTESIAN_POINT('Ctrl Pts',(-98.9086371756676,16.1295634823898,25.0000000000001));
#8977=CARTESIAN_POINT('Ctrl Pts',(-98.8366072848604,16.1669169540907,25.0000000000001));
#8978=CARTESIAN_POINT('Ctrl Pts',(-97.8146405969214,16.6968914317609,25.0000000000001));
#8979=CARTESIAN_POINT('Ctrl Pts',(-96.7996148754077,17.235390438076,25.0000000000001));
#8980=CARTESIAN_POINT('Ctrl Pts',(-95.7917345876971,17.7817475522874,25.0000000000001));
#8981=CARTESIAN_POINT('Ctrl Pts',(-94.7526454700998,18.3450225152184,25.0000000000001));
#8982=CARTESIAN_POINT('Ctrl Pts',(-93.7211510251918,18.9166496466945,25.0000000000001));
#8983=CARTESIAN_POINT('Ctrl Pts',(-92.6974362009878,19.4958587242714,25.0000000000001));
#8984=CARTESIAN_POINT('Ctrl Pts',(-91.6354743167707,20.0967076607488,25.0000000000001));
#8985=CARTESIAN_POINT('Ctrl Pts',(-90.5818840659185,20.7057155131889,25.0000000000001));
#8986=CARTESIAN_POINT('Ctrl Pts',(-89.5368325915886,21.3219821917453,25.0000000000001));
#8987=CARTESIAN_POINT('Ctrl Pts',(-88.4432597431563,21.9668619164451,25.0000000000001));
#8988=CARTESIAN_POINT('Ctrl Pts',(-87.3590367834119,22.6196899704338,25.0000000000001));
#8989=CARTESIAN_POINT('Ctrl Pts',(-86.2843156503055,23.2793942945683,25.0000000000001));
#8990=CARTESIAN_POINT('Ctrl Pts',(-86.1473152047691,23.363490329851,25.0000000000001));
#8991=CARTESIAN_POINT('Ctrl Pts',(-86.0104691157456,23.4476980549826,25.0000000000001));
#8992=CARTESIAN_POINT('Ctrl Pts',(-85.8737776574015,23.5320152073781,25.0000000000001));
#8993=CARTESIAN_POINT('Ctrl Pts',(-85.808653088074,23.5721868340709,25.0000000000001));
#8994=CARTESIAN_POINT('Ctrl Pts',(-85.7435636182602,23.6123832995439,25.0000000000001));
#8995=CARTESIAN_POINT('Ctrl Pts',(-85.6785092769395,23.6526043584145,25.0000000000001));
#8996=CARTESIAN_POINT('Ctrl Pts',(-85.6271072730019,23.6843846052738,25.0000000000001));
#8997=CARTESIAN_POINT('Ctrl Pts',(-85.575725209178,23.716181433953,25.0000000000001));
#8998=CARTESIAN_POINT('Ctrl Pts',(-85.5243537468771,23.748000533409,25.0000000000001));
#8999=CARTESIAN_POINT('Ctrl Pts',(-84.6574156247278,24.2849755209869,25.0000000000001));
#9000=CARTESIAN_POINT('Ctrl Pts',(-83.7942589216096,24.8278271617857,25.0000000000001));
#9001=CARTESIAN_POINT('Ctrl Pts',(-82.9353696413023,25.3758221435343,25.0000000000001));
#9002=CARTESIAN_POINT('Ctrl Pts',(-82.045861072411,25.9433530734819,25.0000000000001));
#9003=CARTESIAN_POINT('Ctrl Pts',(-81.1609294663116,26.5164004546283,25.0000000000001));
#9004=CARTESIAN_POINT('Ctrl Pts',(-80.2810757074104,27.0941097060007,25.0000000000001));
#9005=CARTESIAN_POINT('Ctrl Pts',(-79.3348226214597,27.715416549738,25.0000000000001));
#9006=CARTESIAN_POINT('Ctrl Pts',(-78.3944426985011,28.3421154388075,25.0000000000001));
#9007=CARTESIAN_POINT('Ctrl Pts',(-77.4605156372659,28.9730986607385,25.0000000000001));
#9008=CARTESIAN_POINT('Ctrl Pts',(-76.5849590173578,29.5646454312988,25.0000000000001));
#9009=CARTESIAN_POINT('Ctrl Pts',(-75.715073061572,30.159956917886,25.0000000000001));
#9010=CARTESIAN_POINT('Ctrl Pts',(-74.8513063154526,30.7580902197078,25.0000000000001));
#9011=CARTESIAN_POINT('Ctrl Pts',(-74.4464156532091,31.0384652049367,25.0000000000001));
#9012=CARTESIAN_POINT('Ctrl Pts',(-74.042869183162,31.3194598427701,25.0000000000001));
#9013=CARTESIAN_POINT('Ctrl Pts',(-73.6407113925489,31.600975230648,25.0000000000001));
#9014=CARTESIAN_POINT('Ctrl Pts',(-73.5345264758602,31.6753059752118,25.0000000000001));
#9015=CARTESIAN_POINT('Ctrl Pts',(-73.4284383672046,31.7496730189567,25.0000000000001));
#9016=CARTESIAN_POINT('Ctrl Pts',(-73.3224478746784,31.824074529959,25.0000000000001));
#9017=CARTESIAN_POINT('Ctrl Pts',(-73.2658918473683,31.8637748255974,25.0000000000001));
#9018=CARTESIAN_POINT('Ctrl Pts',(-73.2093636136334,31.9034849348122,25.0000000000001));
#9019=CARTESIAN_POINT('Ctrl Pts',(-73.1528632957563,31.9432045787683,25.0000000000001));
#9020=CARTESIAN_POINT('Ctrl Pts',(-73.1171533786224,31.9683086002598,25.0000000000001));
#9021=CARTESIAN_POINT('Ctrl Pts',(-73.0814546128172,31.9934164305148,25.0000000000001));
#9022=CARTESIAN_POINT('Ctrl Pts',(-73.0457670291454,32.0185279990633,25.0000000000001));
#9023=CARTESIAN_POINT('Ctrl Pts',(-73.0063553520497,32.0462600259806,25.0000000000001));
#9024=CARTESIAN_POINT('Ctrl Pts',(-72.9669507059342,32.0740012593469,25.0000000000001));
#9025=CARTESIAN_POINT('Ctrl Pts',(-72.9275465923938,32.1017562294851,25.0000000000001));
#9026=CARTESIAN_POINT('Ctrl Pts',(-71.754282216512,32.9281653221144,25.0000000000001));
#9027=CARTESIAN_POINT('Ctrl Pts',(-70.5832630059994,33.765499217731,25.0000000000001));
#9028=CARTESIAN_POINT('Ctrl Pts',(-69.4119648391555,34.6144663184202,25.0000000000001));
#9029=CARTESIAN_POINT('Ctrl Pts',(-67.5244483181643,35.9825547127243,25.0000000000001));
#9030=CARTESIAN_POINT('Ctrl Pts',(-65.6362106229917,37.3808549641196,25.0000000000001));
#9031=CARTESIAN_POINT('Ctrl Pts',(-63.736803082023,38.8124625160226,25.0000000000001));
#9032=CARTESIAN_POINT('Ctrl Pts',(-63.1641508526633,39.244077763663,25.0000000000001));
#9033=CARTESIAN_POINT('Ctrl Pts',(-62.5904834077693,39.6787207396113,25.0000000000001));
#9034=CARTESIAN_POINT('Ctrl Pts',(-62.015513259775,40.1164754881207,25.0000000000001));
#9035=CARTESIAN_POINT('Ctrl Pts',(-61.7459960029027,40.3216730264845,25.0000000000001));
#9036=CARTESIAN_POINT('Ctrl Pts',(-61.4761924871871,40.5275542859727,25.0000000000001));
#9037=CARTESIAN_POINT('Ctrl Pts',(-61.2060729689618,40.7341278022368,25.0000000000001));
#9038=CARTESIAN_POINT('Ctrl Pts',(-61.1367061914413,40.7871759464008,25.0000000000001));
#9039=CARTESIAN_POINT('Ctrl Pts',(-61.0673185741674,40.8402697419253,25.0000000000001));
#9040=CARTESIAN_POINT('Ctrl Pts',(-60.9979096122979,40.8934093323168,25.0000000000001));
#9041=CARTESIAN_POINT('Ctrl Pts',(-60.9490449425875,40.9308201862337,25.0000000000001));
#9042=CARTESIAN_POINT('Ctrl Pts',(-60.9001696938147,40.9682537375167,25.0000000000001));
#9043=CARTESIAN_POINT('Ctrl Pts',(-60.8512836896761,41.0057100361011,25.0000000000001));
#9044=CARTESIAN_POINT('Ctrl Pts',(-60.8325758368311,41.0200439325687,25.0000000000001));
#9045=CARTESIAN_POINT('Ctrl Pts',(-60.8138664088997,41.0343811602963,25.0000000000001));
#9046=CARTESIAN_POINT('Ctrl Pts',(-60.7951553959967,41.0487217220779,25.0000000000001));
#9047=CARTESIAN_POINT('Ctrl Pts',(-60.7754197597175,41.0638475793912,25.0000000000001));
#9048=CARTESIAN_POINT('Ctrl Pts',(-60.7556889733333,41.0789720776831,25.0000000000001));
#9049=CARTESIAN_POINT('Ctrl Pts',(-60.7359667875713,41.0940923301713,25.0000000000001));
#9050=CARTESIAN_POINT('Ctrl Pts',(-60.0445237146081,41.6241955332639,25.0000000000001));
#9051=CARTESIAN_POINT('Ctrl Pts',(-59.3621639470488,42.1502148040397,25.0000000000001));
#9052=CARTESIAN_POINT('Ctrl Pts',(-58.6878564666335,42.6724517572262,25.0000000000001));
#9053=CARTESIAN_POINT('Ctrl Pts',(-57.9873078541347,43.2150119149827,25.0000000000001));
#9054=CARTESIAN_POINT('Ctrl Pts',(-57.2954506251931,43.7534898234267,25.0000000000001));
#9055=CARTESIAN_POINT('Ctrl Pts',(-56.6111684755191,44.288264626604,25.0000000000001));
#9056=CARTESIAN_POINT('Ctrl Pts',(-56.205629463576,44.6051982853235,25.0000000000001));
#9057=CARTESIAN_POINT('Ctrl Pts',(-55.8027518035775,44.9208320505127,25.0000000000001));
#9058=CARTESIAN_POINT('Ctrl Pts',(-55.4023089152689,45.2352508066007,25.0000000000001));
#9059=CARTESIAN_POINT('Ctrl Pts',(-55.2146013113743,45.3826345985169,25.0000000000001));
#9060=CARTESIAN_POINT('Ctrl Pts',(-55.0274287488623,45.529751479852,25.0000000000001));
#9061=CARTESIAN_POINT('Ctrl Pts',(-54.8407681811854,45.6766104934432,25.0000000000001));
#9062=CARTESIAN_POINT('Ctrl Pts',(-54.8222267879297,45.6911983132384,25.0000000000001));
#9063=CARTESIAN_POINT('Ctrl Pts',(-54.8036903862308,45.7057836357621,25.0000000000001));
#9064=CARTESIAN_POINT('Ctrl Pts',(-54.7851477621434,45.7203752785472,25.0000000000001));
#9065=CARTESIAN_POINT('Ctrl Pts',(-54.3014372043673,46.1010189046712,25.0000000000001));
#9066=CARTESIAN_POINT('Ctrl Pts',(-53.815452761034,46.4844273276019,25.0000000000001));
#9067=CARTESIAN_POINT('Ctrl Pts',(-53.3318153552279,46.8668393594794,25.0000000000001));
#9068=CARTESIAN_POINT('Ctrl Pts',(-52.793096355682,47.2928044001363,25.0000000000001));
#9069=CARTESIAN_POINT('Ctrl Pts',(-52.2572888932505,47.7175326831695,25.0000000000001));
#9070=CARTESIAN_POINT('Ctrl Pts',(-51.7307337221954,48.1357755371239,25.0000000000001));
#9071=CARTESIAN_POINT('Ctrl Pts',(-51.1509899550892,48.5962661011628,25.0000000000001));
#9072=CARTESIAN_POINT('Ctrl Pts',(-50.5824604036283,49.0488932231173,25.0000000000001));
#9073=CARTESIAN_POINT('Ctrl Pts',(-50.033573635379,49.4866107010153,25.0000000000001));
#9074=CARTESIAN_POINT('Ctrl Pts',(-49.7934356742699,49.6781120975957,25.0000000000001));
#9075=CARTESIAN_POINT('Ctrl Pts',(-49.5570572165051,49.8667593624178,25.0000000000001));
#9076=CARTESIAN_POINT('Ctrl Pts',(-49.3251436624354,50.051961667685,25.0000000000001));
#9077=CARTESIAN_POINT('Ctrl Pts',(-49.2979662928179,50.0736650628335,25.0000000000001));
#9078=CARTESIAN_POINT('Ctrl Pts',(-49.2708502396166,50.0953211487278,25.0000000000001));
#9079=CARTESIAN_POINT('Ctrl Pts',(-49.243796638345,50.116928974649,25.0000000000001));
#9080=CARTESIAN_POINT('Ctrl Pts',(-49.2360887390484,50.1230853064641,25.0000000000001));
#9081=CARTESIAN_POINT('Ctrl Pts',(-49.2283859092831,50.1292377207798,25.0000000000001));
#9082=CARTESIAN_POINT('Ctrl Pts',(-49.2206881753122,50.135386195609,25.0000000000001));
#9083=CARTESIAN_POINT('Ctrl Pts',(-49.2136388166439,50.1410167882612,25.0000000000001));
#9084=CARTESIAN_POINT('Ctrl Pts',(-49.2065859857244,50.1466502639488,25.0000000000001));
#9085=CARTESIAN_POINT('Ctrl Pts',(-49.1995286205646,50.1522874709358,25.0000000000001));
#9086=CARTESIAN_POINT('Ctrl Pts',(-48.5736996895669,50.6521804398544,25.0000000000001));
#9087=CARTESIAN_POINT('Ctrl Pts',(-47.9148954411139,51.1792736794625,25.0000000000001));
#9088=CARTESIAN_POINT('Ctrl Pts',(-47.2031261108418,51.7495555800309,25.0000000000001));
#9089=CARTESIAN_POINT('Ctrl Pts',(-46.7322561076265,52.1268247723569,25.0000000000001));
#9090=CARTESIAN_POINT('Ctrl Pts',(-46.2382071196254,52.5229967428189,25.0000000000001));
#9091=CARTESIAN_POINT('Ctrl Pts',(-45.7151727286514,52.9426877028818,25.0000000000001));
#9092=CARTESIAN_POINT('Ctrl Pts',(-45.2673909231485,53.3019948136441,25.0000000000001));
#9093=CARTESIAN_POINT('Ctrl Pts',(-44.7983649128932,53.6785406963364,25.0000000000001));
#9094=CARTESIAN_POINT('Ctrl Pts',(-44.3044261761361,54.0752003649523,25.0000000000001));
#9095=CARTESIAN_POINT('Ctrl Pts',(-43.9514920159341,54.35862569002,25.0000000000001));
#9096=CARTESIAN_POINT('Ctrl Pts',(-43.5858381908448,54.6523198557899,25.0000000000001));
#9097=CARTESIAN_POINT('Ctrl Pts',(-43.2061138913264,54.9573203095084,25.0000000000001));
#9098=CARTESIAN_POINT('Ctrl Pts',(-43.1230492008067,55.0240391587593,25.0000000000001));
#9099=CARTESIAN_POINT('Ctrl Pts',(-43.0393111656161,55.0912989849344,25.0000000000001));
#9100=CARTESIAN_POINT('Ctrl Pts',(-42.9548855554703,55.159110563518,25.0000000000001));
#9101=CARTESIAN_POINT('Ctrl Pts',(-42.9487467129319,55.16404134936,25.0000000000001));
#9102=CARTESIAN_POINT('Ctrl Pts',(-42.9426034491638,55.1689756836288,25.0000000000001));
#9103=CARTESIAN_POINT('Ctrl Pts',(-42.9364581930475,55.1739116151576,25.0000000000001));
#9104=CARTESIAN_POINT('Ctrl Pts',(-42.4342170449237,55.5773167574626,25.0000000000001));
#9105=CARTESIAN_POINT('Ctrl Pts',(-41.956235985396,55.9612098550919,25.0000000000001));
#9106=CARTESIAN_POINT('Ctrl Pts',(-41.5020206332019,56.3258915173201,25.0000000000001));
#9107=CARTESIAN_POINT('Ctrl Pts',(-40.9919258908233,56.735437776921,25.0000000000001));
#9108=CARTESIAN_POINT('Ctrl Pts',(-40.5118042106407,57.1207550280515,25.0000000000001));
#9109=CARTESIAN_POINT('Ctrl Pts',(-40.0610034128949,57.4823195544779,25.0000000000001));
#9110=CARTESIAN_POINT('Ctrl Pts',(-39.5686598282259,57.8772034498039,25.0000000000001));
#9111=CARTESIAN_POINT('Ctrl Pts',(-39.1112908860053,58.2437558219308,25.0000000000001));
#9112=CARTESIAN_POINT('Ctrl Pts',(-38.6880935424586,58.5826469939407,25.0000000000001));
#9113=CARTESIAN_POINT('Ctrl Pts',(-38.1712113731884,58.9965598098081,25.0000000000001));
#9114=CARTESIAN_POINT('Ctrl Pts',(-37.7053057014659,59.3692096416051,25.0000000000001));
#9115=CARTESIAN_POINT('Ctrl Pts',(-37.2889677026751,59.7018784459919,25.0000000000001));
#9116=CARTESIAN_POINT('Ctrl Pts',(-37.1898413829962,59.7810838856746,25.0000000000001));
#9117=CARTESIAN_POINT('Ctrl Pts',(-37.0935250781658,59.8580230943006,25.0000000000001));
#9118=CARTESIAN_POINT('Ctrl Pts',(-37.,59.9327136539873,25.0000000000001));
#9119=CARTESIAN_POINT('Origin',(-85.4296283056384,23.8067054410607,25.0000000000001));
#9120=CARTESIAN_POINT('',(65.6680057154831,-5.,25.0000000000001));
#9121=CARTESIAN_POINT('',(20.,72.1122755947453,25.0000000000001));
#9122=CARTESIAN_POINT('',(20.,72.1122755947453,25.0000000000001));
#9123=CARTESIAN_POINT('',(37.,59.9327136539873,25.0000000000001));
#9124=CARTESIAN_POINT('Origin',(5.94655548926424E-16,26.2427388041954,25.0000000000001));
#9125=CARTESIAN_POINT('Ctrl Pts',(37.,59.9327136539873,25.0000000000001));
#9126=CARTESIAN_POINT('Ctrl Pts',(37.379667023306,59.6295057548716,25.0000000000001));
#9127=CARTESIAN_POINT('Ctrl Pts',(37.8053353012187,59.2892352085535,25.0000000000001));
#9128=CARTESIAN_POINT('Ctrl Pts',(38.2782656703118,58.9107382150177,25.0000000000001));
#9129=CARTESIAN_POINT('Ctrl Pts',(38.6687156895296,58.5982521323764,25.0000000000001));
#9130=CARTESIAN_POINT('Ctrl Pts',(39.0913794549942,58.2597099653507,25.0000000000001));
#9131=CARTESIAN_POINT('Ctrl Pts',(39.5469874492648,57.8944807883205,25.0000000000001));
#9132=CARTESIAN_POINT('Ctrl Pts',(39.9543075803571,57.5679606259497,25.0000000000001));
#9133=CARTESIAN_POINT('Ctrl Pts',(40.3879583984683,57.2201102048173,25.0000000000001));
#9134=CARTESIAN_POINT('Ctrl Pts',(40.8484865188096,56.8505053738539,25.0000000000001));
#9135=CARTESIAN_POINT('Ctrl Pts',(41.2999783576224,56.4881527673678,25.0000000000001));
#9136=CARTESIAN_POINT('Ctrl Pts',(41.777302381718,56.1048903670244,25.0000000000001));
#9137=CARTESIAN_POINT('Ctrl Pts',(42.2810069638633,55.7003537526117,25.0000000000001));
#9138=CARTESIAN_POINT('Ctrl Pts',(42.4049655133756,55.6007998201585,25.0000000000001));
#9139=CARTESIAN_POINT('Ctrl Pts',(42.5305219159893,55.4999576756661,25.0000000000001));
#9140=CARTESIAN_POINT('Ctrl Pts',(42.6576847433865,55.3978223055861,25.0000000000001));
#9141=CARTESIAN_POINT('Ctrl Pts',(42.7210177921879,55.3469541036908,25.0000000000001));
#9142=CARTESIAN_POINT('Ctrl Pts',(42.7847493184706,55.2957651191222,25.0000000000001));
#9143=CARTESIAN_POINT('Ctrl Pts',(42.8488803978488,55.2442547498818,25.0000000000001));
#9144=CARTESIAN_POINT('Ctrl Pts',(42.8670093092844,55.2296935272885,25.0000000000001));
#9145=CARTESIAN_POINT('Ctrl Pts',(42.885170149462,55.21510662261,25.0000000000001));
#9146=CARTESIAN_POINT('Ctrl Pts',(42.9033629428465,55.2004940224215,25.0000000000001));
#9147=CARTESIAN_POINT('Ctrl Pts',(42.9117835396531,55.1937305303132,25.0000000000001));
#9148=CARTESIAN_POINT('Ctrl Pts',(42.9202109819016,55.1869615333721,25.0000000000001));
#9149=CARTESIAN_POINT('Ctrl Pts',(42.9286452720233,55.1801870302728,25.0000000000001));
#9150=CARTESIAN_POINT('Ctrl Pts',(42.9355167001405,55.1746678329952,25.0000000000001));
#9151=CARTESIAN_POINT('Ctrl Pts',(42.9423940941063,55.169143839983,25.0000000000001));
#9152=CARTESIAN_POINT('Ctrl Pts',(42.949264125121,55.1636257574225,25.0000000000001));
#9153=CARTESIAN_POINT('Ctrl Pts',(43.4538066664403,54.7583717793348,25.0000000000001));
#9154=CARTESIAN_POINT('Ctrl Pts',(43.9338047887228,54.3728188661298,25.0000000000001));
#9155=CARTESIAN_POINT('Ctrl Pts',(44.3922742549877,54.0046546909899,25.0000000000001));
#9156=CARTESIAN_POINT('Ctrl Pts',(44.9182289894069,53.5822979034466,25.0000000000001));
#9157=CARTESIAN_POINT('Ctrl Pts',(45.4158501546012,53.1828251430864,25.0000000000001));
#9158=CARTESIAN_POINT('Ctrl Pts',(45.8896418211895,52.8027007016266,25.0000000000001));
#9159=CARTESIAN_POINT('Ctrl Pts',(46.5104671522248,52.3046107206372,25.0000000000001));
#9160=CARTESIAN_POINT('Ctrl Pts',(47.0903771812918,51.8397403801932,25.0000000000001));
#9161=CARTESIAN_POINT('Ctrl Pts',(47.6394345771857,51.4000748549018,25.0000000000001));
#9162=CARTESIAN_POINT('Ctrl Pts',(47.9907462386239,51.1187570412772,25.0000000000001));
#9163=CARTESIAN_POINT('Ctrl Pts',(48.3294254446928,50.8477570196711,25.0000000000001));
#9164=CARTESIAN_POINT('Ctrl Pts',(48.6581018226499,50.5849711025823,25.0000000000001));
#9165=CARTESIAN_POINT('Ctrl Pts',(48.8198722274257,50.4556311590152,25.0000000000001));
#9166=CARTESIAN_POINT('Ctrl Pts',(48.9792194319725,50.3282810641903,25.0000000000001));
#9167=CARTESIAN_POINT('Ctrl Pts',(49.1364569454656,50.2026700971239,25.0000000000001));
#9168=CARTESIAN_POINT('Ctrl Pts',(49.1559822657899,50.1870720740203,25.0000000000001));
#9169=CARTESIAN_POINT('Ctrl Pts',(49.1754750548033,50.1715008684445,25.0000000000001));
#9170=CARTESIAN_POINT('Ctrl Pts',(49.194935912914,50.1559560004978,25.0000000000001));
#9171=CARTESIAN_POINT('Ctrl Pts',(49.2026425963922,50.1498000860826,25.0000000000001));
#9172=CARTESIAN_POINT('Ctrl Pts',(49.2103442723557,50.1436483020264,25.0000000000001));
#9173=CARTESIAN_POINT('Ctrl Pts',(49.2180409780931,50.1375006185279,25.0000000000001));
#9174=CARTESIAN_POINT('Ctrl Pts',(49.2253110938493,50.1316936704398,25.0000000000001));
#9175=CARTESIAN_POINT('Ctrl Pts',(49.2325829791765,50.1258854254269,25.0000000000001));
#9176=CARTESIAN_POINT('Ctrl Pts',(49.2398606897643,50.1200726448833,25.0000000000001));
#9177=CARTESIAN_POINT('Ctrl Pts',(49.8606042856743,49.6242785001005,25.0000000000001));
#9178=CARTESIAN_POINT('Ctrl Pts',(50.5142825462621,49.1030328807307,25.0000000000001));
#9179=CARTESIAN_POINT('Ctrl Pts',(51.1871655721719,48.567830362299,25.0000000000001));
#9180=CARTESIAN_POINT('Ctrl Pts',(51.7158663366829,48.1473085631639,25.0000000000001));
#9181=CARTESIAN_POINT('Ctrl Pts',(52.2564249707963,47.7181716623712,25.0000000000001));
#9182=CARTESIAN_POINT('Ctrl Pts',(52.8021626903985,47.2859712302726,25.0000000000001));
#9183=CARTESIAN_POINT('Ctrl Pts',(53.2807819115689,46.9069257167037,25.0000000000001));
#9184=CARTESIAN_POINT('Ctrl Pts',(53.7633851027738,46.5255242814923,25.0000000000001));
#9185=CARTESIAN_POINT('Ctrl Pts',(54.2454397069039,46.1454810332774,25.0000000000001));
#9186=CARTESIAN_POINT('Ctrl Pts',(54.4068021109733,46.0182657932259,25.0000000000001));
#9187=CARTESIAN_POINT('Ctrl Pts',(54.5681027698807,45.8912024350973,25.0000000000001));
#9188=CARTESIAN_POINT('Ctrl Pts',(54.729170760509,45.7644292654329,25.0000000000001));
#9189=CARTESIAN_POINT('Ctrl Pts',(54.7576244445241,45.7420339794598,25.0000000000001));
#9190=CARTESIAN_POINT('Ctrl Pts',(54.7860708662357,45.7196477481137,25.0000000000001));
#9191=CARTESIAN_POINT('Ctrl Pts',(54.8145090816246,45.6972713320229,25.0000000000001));
#9192=CARTESIAN_POINT('Ctrl Pts',(54.8348702776094,45.6812502636389,25.0000000000001));
#9193=CARTESIAN_POINT('Ctrl Pts',(54.8552330883136,45.6652296458008,25.0000000000001));
#9194=CARTESIAN_POINT('Ctrl Pts',(54.8756040257786,45.6492043660801,25.0000000000001));
#9195=CARTESIAN_POINT('Ctrl Pts',(55.5550265500445,45.1147205693163,25.0000000000001));
#9196=CARTESIAN_POINT('Ctrl Pts',(56.2412452453015,44.5768116431681,25.0000000000001));
#9197=CARTESIAN_POINT('Ctrl Pts',(56.9353824441227,44.0350550110448,25.0000000000001));
#9198=CARTESIAN_POINT('Ctrl Pts',(57.5651721195718,43.5435200031287,25.0000000000001));
#9199=CARTESIAN_POINT('Ctrl Pts',(58.2014803619766,43.048817738353,25.0000000000001));
#9200=CARTESIAN_POINT('Ctrl Pts',(58.8451714214353,42.5506593941846,25.0000000000001));
#9201=CARTESIAN_POINT('Ctrl Pts',(59.4687471352858,42.0680684982715,25.0000000000001));
#9202=CARTESIAN_POINT('Ctrl Pts',(60.0992513234504,41.5822340273024,25.0000000000001));
#9203=CARTESIAN_POINT('Ctrl Pts',(60.7374957459951,41.0929201403882,25.0000000000001));
#9204=CARTESIAN_POINT('Ctrl Pts',(60.7575133230696,41.0775735457312,25.0000000000001));
#9205=CARTESIAN_POINT('Ctrl Pts',(60.7775403998995,41.0622220872218,25.0000000000001));
#9206=CARTESIAN_POINT('Ctrl Pts',(60.7975709297175,41.0468704118127,25.0000000000001));
#9207=CARTESIAN_POINT('Ctrl Pts',(62.1358201086493,40.0212177107564,25.0000000000001));
#9208=CARTESIAN_POINT('Ctrl Pts',(63.4659680993238,39.012623086552,25.0000000000001));
#9209=CARTESIAN_POINT('Ctrl Pts',(64.791604272834,38.0200398160107,25.0000000000001));
#9210=CARTESIAN_POINT('Ctrl Pts',(66.1951427752259,36.9691264018528,25.0000000000001));
#9211=CARTESIAN_POINT('Ctrl Pts',(67.5936194820664,35.9361573083481,25.0000000000001));
#9212=CARTESIAN_POINT('Ctrl Pts',(68.9912744880311,34.9198762099585,25.0000000000001));
#9213=CARTESIAN_POINT('Ctrl Pts',(70.0407792639522,34.1567466380065,25.0000000000001));
#9214=CARTESIAN_POINT('Ctrl Pts',(71.0898199054102,33.4030260188376,25.0000000000001));
#9215=CARTESIAN_POINT('Ctrl Pts',(72.1402068924224,32.6581999429906,25.0000000000001));
#9216=CARTESIAN_POINT('Ctrl Pts',(72.3863913425034,32.4836313314639,25.0000000000001));
#9217=CARTESIAN_POINT('Ctrl Pts',(72.6326498509789,32.3095514218598,25.0000000000001));
#9218=CARTESIAN_POINT('Ctrl Pts',(72.8790059372784,32.1359538175003,25.0000000000001));
#9219=CARTESIAN_POINT('Ctrl Pts',(72.9286909378154,32.1009427195591,25.0000000000001));
#9220=CARTESIAN_POINT('Ctrl Pts',(72.9783799076115,32.0659512395566,25.0000000000001));
#9221=CARTESIAN_POINT('Ctrl Pts',(73.0280730400874,32.030979325534,25.0000000000001));
#9222=CARTESIAN_POINT('Ctrl Pts',(73.0635665772672,32.0060004830105,25.0000000000001));
#9223=CARTESIAN_POINT('Ctrl Pts',(73.0990697832648,31.9810263118437,25.0000000000001));
#9224=CARTESIAN_POINT('Ctrl Pts',(73.1345847051824,31.9560554193695,25.0000000000001));
#9225=CARTESIAN_POINT('Ctrl Pts',(74.1000277183134,31.2772428986274,25.0000000000001));
#9226=CARTESIAN_POINT('Ctrl Pts',(75.0736303041406,30.6012086898854,25.0000000000001));
#9227=CARTESIAN_POINT('Ctrl Pts',(76.0547670744571,29.9293290727267,25.0000000000001));
#9228=CARTESIAN_POINT('Ctrl Pts',(76.9745827966288,29.2994419316403,25.0000000000001));
#9229=CARTESIAN_POINT('Ctrl Pts',(77.9010206378247,28.6732065536317,25.0000000000001));
#9230=CARTESIAN_POINT('Ctrl Pts',(78.8335336207789,28.0517239817985,25.0000000000001));
#9231=CARTESIAN_POINT('Ctrl Pts',(79.7077645422984,27.4690840707048,25.0000000000001));
#9232=CARTESIAN_POINT('Ctrl Pts',(80.5873350480293,26.8906215256502,25.0000000000001));
#9233=CARTESIAN_POINT('Ctrl Pts',(81.4717631628992,26.3172112524276,25.0000000000001));
#9234=CARTESIAN_POINT('Ctrl Pts',(82.3009145205897,25.7796391212815,25.0000000000001));
#9235=CARTESIAN_POINT('Ctrl Pts',(83.1343352590044,25.2465074533943,25.0000000000001));
#9236=CARTESIAN_POINT('Ctrl Pts',(83.9715992196895,24.7185072927335,25.0000000000001));
#9237=CARTESIAN_POINT('Ctrl Pts',(84.3640667012607,24.4710072174237,25.0000000000001));
#9238=CARTESIAN_POINT('Ctrl Pts',(84.7573782112601,24.2246342293148,25.0000000000001));
#9239=CARTESIAN_POINT('Ctrl Pts',(85.151487452235,23.9794570370164,25.0000000000001));
#9240=CARTESIAN_POINT('Ctrl Pts',(85.2759172916967,23.9020486550107,25.0000000000001));
#9241=CARTESIAN_POINT('Ctrl Pts',(85.4004266383056,23.8247594596692,25.0000000000001));
#9242=CARTESIAN_POINT('Ctrl Pts',(85.5250140009801,23.7475915785448,25.0000000000001));
#9243=CARTESIAN_POINT('Ctrl Pts',(85.6006832213009,23.7007229935363,25.0000000000001));
#9244=CARTESIAN_POINT('Ctrl Pts',(85.6763761818179,23.6539022640716,25.0000000000001));
#9245=CARTESIAN_POINT('Ctrl Pts',(85.7521211486376,23.6071122170034,25.0000000000001));
#9246=CARTESIAN_POINT('Ctrl Pts',(86.8189992193685,22.9480680951102,25.0000000000001));
#9247=CARTESIAN_POINT('Ctrl Pts',(87.8953183319792,22.2956602946924,25.0000000000001));
#9248=CARTESIAN_POINT('Ctrl Pts',(88.9809339474695,21.6509533357167,25.0000000000001));
#9249=CARTESIAN_POINT('Ctrl Pts',(90.0187858805737,21.0346114610132,25.0000000000001));
#9250=CARTESIAN_POINT('Ctrl Pts',(91.0651344673981,20.4253078932095,25.0000000000001));
#9251=CARTESIAN_POINT('Ctrl Pts',(92.1198205279235,19.8239389045421,25.0000000000001));
#9252=CARTESIAN_POINT('Ctrl Pts',(93.1371001567188,19.2438986020696,25.0000000000001));
#9253=CARTESIAN_POINT('Ctrl Pts',(94.162136490687,18.6712401789023,25.0000000000001));
#9254=CARTESIAN_POINT('Ctrl Pts',(95.1947529130522,18.1067332667718,25.0000000000001));
#9255=CARTESIAN_POINT('Ctrl Pts',(96.196944163343,17.5588590747557,25.0000000000001));
#9256=CARTESIAN_POINT('Ctrl Pts',(97.2062755267639,17.0186632391373,25.0000000000001));
#9257=CARTESIAN_POINT('Ctrl Pts',(98.2225511036303,16.4868141437658,25.0000000000001));
#9258=CARTESIAN_POINT('Ctrl Pts',(98.4885714663643,16.3475972891142,25.0000000000001));
#9259=CARTESIAN_POINT('Ctrl Pts',(98.7550674415586,16.2089521416587,25.0000000000001));
#9260=CARTESIAN_POINT('Ctrl Pts',(99.0220350938054,16.0708902585445,25.0000000000001));
#9261=CARTESIAN_POINT('Ctrl Pts',(99.0971646665005,16.0320371233554,25.0000000000001));
#9262=CARTESIAN_POINT('Ctrl Pts',(99.1723388929282,15.9932264015618,25.0000000000001));
#9263=CARTESIAN_POINT('Ctrl Pts',(99.2475623772724,15.9544559749396,25.0000000000001));
#9264=CARTESIAN_POINT('Ctrl Pts',(100.299373993986,15.41234887286,25.0000000000001));
#9265=CARTESIAN_POINT('Ctrl Pts',(101.360529515776,14.8782723788936,25.0000000000001));
#9266=CARTESIAN_POINT('Ctrl Pts',(102.430907202419,14.3529815560378,25.0000000000001));
#9267=CARTESIAN_POINT('Ctrl Pts',(103.473274291026,13.8414370119714,25.0000000000001));
#9268=CARTESIAN_POINT('Ctrl Pts',(104.52438733127,13.3382244702285,25.0000000000001));
#9269=CARTESIAN_POINT('Ctrl Pts',(105.584100597309,12.8440072383845,25.0000000000001));
#9270=CARTESIAN_POINT('Ctrl Pts',(106.619814754682,12.360982442675,25.0000000000001));
#9271=CARTESIAN_POINT('Ctrl Pts',(107.663744132073,11.8865502575117,25.0000000000001));
#9272=CARTESIAN_POINT('Ctrl Pts',(108.715718557623,11.4212951390412,25.0000000000001));
#9273=CARTESIAN_POINT('Ctrl Pts',(109.74685733301,10.965254971666,25.0000000000001));
#9274=CARTESIAN_POINT('Ctrl Pts',(110.78572573032,10.5180320455846,25.0000000000001));
#9275=CARTESIAN_POINT('Ctrl Pts',(111.832128697192,10.0801413425618,25.0000000000001));
#9276=CARTESIAN_POINT('Ctrl Pts',(112.11045009164,9.96367153605378,25.0000000000001));
#9277=CARTESIAN_POINT('Ctrl Pts',(112.389304320048,9.8478617348605,25.0000000000001));
#9278=CARTESIAN_POINT('Ctrl Pts',(112.668687272398,9.73272118180913,25.0000000000001));
#9279=CARTESIAN_POINT('Ctrl Pts',(112.799648031312,9.6787490475663,25.0000000000001));
#9280=CARTESIAN_POINT('Ctrl Pts',(112.930724962206,9.62492396215648,25.0000000000001));
#9281=CARTESIAN_POINT('Ctrl Pts',(113.061917627266,9.57124686282096,25.0000000000001));
#9282=CARTESIAN_POINT('Ctrl Pts',(113.136076136524,9.54090512331734,25.0000000000001));
#9283=CARTESIAN_POINT('Ctrl Pts',(113.210271625404,9.51061066867802,25.0000000000001));
#9284=CARTESIAN_POINT('Ctrl Pts',(113.284504013508,9.4803636668373,25.0000000000001));
#9285=CARTESIAN_POINT('Ctrl Pts',(113.332364618527,9.4608622087127,25.0000000000001));
#9286=CARTESIAN_POINT('Ctrl Pts',(113.38023826595,9.44138140910595,25.0000000000001));
#9287=CARTESIAN_POINT('Ctrl Pts',(113.428132494267,9.4219182412191,25.0000000000001));
#9288=CARTESIAN_POINT('Ctrl Pts',(114.149202999218,9.12889094358361,25.0000000000001));
#9289=CARTESIAN_POINT('Ctrl Pts',(114.875975859862,8.83944349063256,25.0000000000001));
#9290=CARTESIAN_POINT('Ctrl Pts',(115.60777575188,8.55405656223017,25.0000000000001));
#9291=CARTESIAN_POINT('Ctrl Pts',(116.328331424398,8.27305464850276,25.0000000000001));
#9292=CARTESIAN_POINT('Ctrl Pts',(117.053760911735,7.99598951491613,25.0000000000001));
#9293=CARTESIAN_POINT('Ctrl Pts',(117.783384155275,7.72328397406765,25.0000000000001));
#9294=CARTESIAN_POINT('Ctrl Pts',(118.498966389033,7.45582643100485,25.0000000000001));
#9295=CARTESIAN_POINT('Ctrl Pts',(119.218582550737,7.19256232969555,25.0000000000001));
#9296=CARTESIAN_POINT('Ctrl Pts',(119.941556034713,6.9338548568966,25.0000000000001));
#9297=CARTESIAN_POINT('Ctrl Pts',(120.657883223477,6.67752568188564,25.0000000000001));
#9298=CARTESIAN_POINT('Ctrl Pts',(121.377506358092,6.42566980935821,25.0000000000001));
#9299=CARTESIAN_POINT('Ctrl Pts',(122.099731764364,6.1786043370424,25.0000000000001));
#9300=CARTESIAN_POINT('Ctrl Pts',(122.813510112138,5.93442851175294,25.0000000000001));
#9301=CARTESIAN_POINT('Ctrl Pts',(123.529830247605,5.69493171691093,25.0000000000001));
#9302=CARTESIAN_POINT('Ctrl Pts',(124.24798695059,5.46038386773084,25.0000000000001));
#9303=CARTESIAN_POINT('Ctrl Pts',(124.724609977416,5.30472020080811,25.0000000000001));
#9304=CARTESIAN_POINT('Ctrl Pts',(125.20204121732,5.15123562927839,25.0000000000001));
#9305=CARTESIAN_POINT('Ctrl Pts',(125.680065601264,5.,25.0000000000001));
#9306=CARTESIAN_POINT('Origin',(-85.4296283056384,23.8067054410608,-48.9999999999999));
#9307=CARTESIAN_POINT('',(-65.6680057154831,-5.,-48.9999999999999));
#9308=CARTESIAN_POINT('',(-20.,72.1122755947453,-48.9999999999999));
#9309=CARTESIAN_POINT('Ctrl Pts',(-37.,59.9327136539873,-48.9999999999999));
#9310=CARTESIAN_POINT('Ctrl Pts',(-63.6931530394793,38.6151528518972,-48.9999999999999));
#9311=CARTESIAN_POINT('Ctrl Pts',(-89.434492138698,16.4672437123984,-48.9999999999999));
#9312=CARTESIAN_POINT('Ctrl Pts',(-125.680065601287,4.99999999999283,-48.9999999999999));
#9313=CARTESIAN_POINT('Origin',(-85.4296283056384,23.8067054410608,-48.9999999999999));
#9314=CARTESIAN_POINT('',(20.,-5.,-48.9999999999999));
#9315=CARTESIAN_POINT('',(65.6680057154831,-5.,-48.9999999999999));
#9316=CARTESIAN_POINT('Ctrl Pts',(125.680065601293,4.99999999999088,-49.));
#9317=CARTESIAN_POINT('Ctrl Pts',(89.4344921387009,16.4672437123958,-49.));
#9318=CARTESIAN_POINT('Ctrl Pts',(63.6931530394808,38.615152851896,-48.9999999999999));
#9319=CARTESIAN_POINT('Ctrl Pts',(37.,59.9327136539873,-48.9999999999999));
#9320=CARTESIAN_POINT('Origin',(-145.859521458148,-5.,-58.9999999999999));
#9321=CARTESIAN_POINT('',(-145.859521458148,1.99649259469911E-14,-58.9999999999999));
#9322=CARTESIAN_POINT('Ctrl Pts',(-145.859521458148,2.04281036531029E-14,
-58.9999999999999));
#9323=CARTESIAN_POINT('Ctrl Pts',(-138.765903145325,1.29386700366004,-58.9999999999999));
#9324=CARTESIAN_POINT('Ctrl Pts',(-132.060245856665,2.9814615985512,-58.9999999999999));
#9325=CARTESIAN_POINT('Ctrl Pts',(-125.680065601889,4.99999999980248,-58.9999999999999));
#9326=CARTESIAN_POINT('',(-145.859521458148,1.99493199737333E-14,-58.9999999999999));
#9327=CARTESIAN_POINT('Origin',(-145.859521458148,-5.,-58.9999999999999));
#9328=CARTESIAN_POINT('',(145.859521458148,1.99493199737333E-14,-59.));
#9329=CARTESIAN_POINT('',(145.859521458148,1.99493199737333E-14,-59.));
#9330=CARTESIAN_POINT('Ctrl Pts',(145.859521458148,1.99966320462804E-14,
-59.));
#9331=CARTESIAN_POINT('Ctrl Pts',(139.935495507955,1.08053483677362,-59.));
#9332=CARTESIAN_POINT('Ctrl Pts',(134.282043748658,2.43566561952013,-59.));
#9333=CARTESIAN_POINT('Ctrl Pts',(127.792835858247,4.34336551753063,-59.));
#9334=CARTESIAN_POINT('Ctrl Pts',(126.732026641956,4.6671843627512,-59.));
#9335=CARTESIAN_POINT('Ctrl Pts',(125.68006560189,4.99999999980207,-59.));
#9336=CARTESIAN_POINT('Origin',(-145.859521458148,-5.,144.542028553823));
#9337=CARTESIAN_POINT('',(-145.859521458148,0.,35.0000000000001));
#9338=CARTESIAN_POINT('',(-36.8276756314269,0.,133.982075177761));
#9339=CARTESIAN_POINT('Ctrl Pts',(-145.859521458148,8.23993651088983E-17,
35.0000000000001));
#9340=CARTESIAN_POINT('Ctrl Pts',(-145.635702363577,0.000231282962457004,
35.0000000000001));
#9341=CARTESIAN_POINT('Ctrl Pts',(-145.411883255014,0.000447783512624677,
35.0006859694096));
#9342=CARTESIAN_POINT('Ctrl Pts',(-145.188067286082,0.000650024992512574,
35.0020579084857));
#9343=CARTESIAN_POINT('Ctrl Pts',(-139.052999252432,0.00619371004421888,
35.0396644278488));
#9344=CARTESIAN_POINT('Ctrl Pts',(-132.962545444182,-5.00267456489816E-15,
35.5922856589093));
#9345=CARTESIAN_POINT('Ctrl Pts',(-126.977116946521,5.75982404132925E-15,
36.6397078209221));
#9346=CARTESIAN_POINT('Ctrl Pts',(-123.729336577937,-8.83548270628736E-15,
37.2080542871332));
#9347=CARTESIAN_POINT('Ctrl Pts',(-120.512481495569,6.22417271669332E-15,
37.9221153240664));
#9348=CARTESIAN_POINT('Ctrl Pts',(-117.336234309904,2.03055396797011E-14,
38.7787168150856));
#9349=CARTESIAN_POINT('Ctrl Pts',(-114.085205078277,2.1960099348902E-14,
39.6554862616599));
#9350=CARTESIAN_POINT('Ctrl Pts',(-110.876720955834,-3.26284544765647E-14,
40.6815897913547));
#9351=CARTESIAN_POINT('Ctrl Pts',(-107.721164151354,-1.36321397827812E-14,
41.8535592808524));
#9352=CARTESIAN_POINT('Ctrl Pts',(-104.5107545404,-2.00540520775008E-14,
43.0459010277944));
#9353=CARTESIAN_POINT('Ctrl Pts',(-101.355129960869,-4.96859830016179E-14,
44.3892216824941));
#9354=CARTESIAN_POINT('Ctrl Pts',(-98.2651875381795,-8.7145968338722E-15,
45.8797997202868));
#9355=CARTESIAN_POINT('Ctrl Pts',(-95.1416080119443,2.68306712685109E-14,
47.3866041859354));
#9356=CARTESIAN_POINT('Ctrl Pts',(-92.0851458120305,-2.46012083690602E-14,
49.0438828741843));
#9357=CARTESIAN_POINT('Ctrl Pts',(-89.1070253835134,-4.47091941648079E-15,
50.8477906894533));
#9358=CARTESIAN_POINT('Ctrl Pts',(-86.116852734007,1.31897776828331E-14,
52.6589987788904));
#9359=CARTESIAN_POINT('Ctrl Pts',(-83.2056472832304,-2.52433361746903E-14,
54.6180166790272));
#9360=CARTESIAN_POINT('Ctrl Pts',(-80.384830163582,-3.25227617460708E-14,
56.7210696683281));
#9361=CARTESIAN_POINT('Ctrl Pts',(-77.5611534148143,-5.45739529723217E-14,
58.8262546468053));
#9362=CARTESIAN_POINT('Ctrl Pts',(-74.838114010143,-1.58426147313227E-14,
61.0685191399763));
#9363=CARTESIAN_POINT('Ctrl Pts',(-72.2297132774974,-3.95963338885915E-14,
63.4364962704633));
#9364=CARTESIAN_POINT('Ctrl Pts',(-69.6213194790221,-7.79039001579624E-14,
65.8044671059218));
#9365=CARTESIAN_POINT('Ctrl Pts',(-67.1275347240086,-6.25228860961752E-14,
68.2980716005042));
#9366=CARTESIAN_POINT('Ctrl Pts',(-64.7594023581045,-8.88178419700125E-14,
70.9062580231546));
#9367=CARTESIAN_POINT('Ctrl Pts',(-62.4021012990926,-9.12248625477642E-14,
73.5025151854382));
#9368=CARTESIAN_POINT('Ctrl Pts',(-60.169846560561,-4.0610067571623E-14,
76.2117317741152));
#9369=CARTESIAN_POINT('Ctrl Pts',(-58.0726499521868,-6.27156238454472E-14,
79.0216408040367));
#9370=CARTESIAN_POINT('Ctrl Pts',(-55.9948328500291,-7.60233291321462E-14,
81.8055843859426));
#9371=CARTESIAN_POINT('Ctrl Pts',(-54.0490749518655,-1.67744203884114E-13,
84.6891394721334));
#9372=CARTESIAN_POINT('Ctrl Pts',(-52.2449416359332,-1.38934194302791E-13,
87.6582306461879));
#9373=CARTESIAN_POINT('Ctrl Pts',(-50.4652489916243,-1.05237142154808E-13,
90.5870994144124));
#9374=CARTESIAN_POINT('Ctrl Pts',(-48.8232383526347,-1.1932076725731E-13,
93.5993053079782));
#9375=CARTESIAN_POINT('Ctrl Pts',(-47.3258881353928,-1.2706433568353E-13,
96.6820335276708));
#9376=CARTESIAN_POINT('Ctrl Pts',(-45.855086603224,-1.35827824389417E-13,
99.7101036054481));
#9377=CARTESIAN_POINT('Ctrl Pts',(-44.5237168473912,-7.3722747694714E-14,
102.806759783349));
#9378=CARTESIAN_POINT('Ctrl Pts',(-43.3384647873198,-7.32425154326057E-14,
105.955904638828));
#9379=CARTESIAN_POINT('Ctrl Pts',(-42.1784113697529,-6.02896671181379E-14,
109.038098186581));
#9380=CARTESIAN_POINT('Ctrl Pts',(-41.1578799651057,-1.27995749366182E-13,
112.171204882295));
#9381=CARTESIAN_POINT('Ctrl Pts',(-40.2800279987792,-1.24975527024613E-13,
115.345683225176));
#9382=CARTESIAN_POINT('Ctrl Pts',(-38.5944013814798,-1.62104376724653E-13,
121.441227116469));
#9383=CARTESIAN_POINT('Ctrl Pts',(-37.4373840532588,-5.41978339669594E-15,
127.68681682945));
#9384=CARTESIAN_POINT('Ctrl Pts',(-36.8276756314269,-1.16656359051837E-13,
133.982075177761));
#9385=CARTESIAN_POINT('',(-145.859521458148,-5.,35.0000000000001));
#9386=CARTESIAN_POINT('',(-36.8276756314269,-5.,133.982075177761));
#9387=CARTESIAN_POINT('Origin',(145.859521458148,-5.,144.542028553823));
#9388=CARTESIAN_POINT('',(145.859521458148,6.34121985785824E-17,35.0000000000001));
#9389=CARTESIAN_POINT('',(36.827675631427,0.,133.982075177761));
#9390=CARTESIAN_POINT('Ctrl Pts',(145.859521458148,3.17060992892912E-17,
35.0000000000001));
#9391=CARTESIAN_POINT('Ctrl Pts',(145.635702363633,0.000231282959717141,
35.0000000000001));
#9392=CARTESIAN_POINT('Ctrl Pts',(145.41188325512,0.000447783510709151,
35.0006859694093));
#9393=CARTESIAN_POINT('Ctrl Pts',(145.18806728624,0.00065002499126718,35.0020579084847));
#9394=CARTESIAN_POINT('Ctrl Pts',(139.052999252553,0.00619371003938468,
35.0396644278391));
#9395=CARTESIAN_POINT('Ctrl Pts',(132.962545444248,2.81306248191126E-14,
35.5922856588977));
#9396=CARTESIAN_POINT('Ctrl Pts',(126.977116946521,-1.25959050860987E-14,
36.6397078209221));
#9397=CARTESIAN_POINT('Ctrl Pts',(123.729336577941,-1.22807761130853E-14,
37.2080542871325));
#9398=CARTESIAN_POINT('Ctrl Pts',(120.512481495573,-2.84858070297575E-14,
37.9221153240654));
#9399=CARTESIAN_POINT('Ctrl Pts',(117.336234309904,1.86685976871553E-14,
38.7787168150856));
#9400=CARTESIAN_POINT('Ctrl Pts',(114.08520507828,4.21595021817856E-14,
39.6554862616589));
#9401=CARTESIAN_POINT('Ctrl Pts',(110.876720955837,-1.07034139801461E-15,
40.6815897913534));
#9402=CARTESIAN_POINT('Ctrl Pts',(107.721164151354,-3.37470208163848E-14,
41.8535592808524));
#9403=CARTESIAN_POINT('Ctrl Pts',(104.510754540403,-4.76367518704849E-14,
43.0459010277931));
#9404=CARTESIAN_POINT('Ctrl Pts',(101.355129960872,-3.43757017307364E-14,
44.3892216824924));
#9405=CARTESIAN_POINT('Ctrl Pts',(98.2651875381796,-2.63709732083997E-14,
45.8797997202868));
#9406=CARTESIAN_POINT('Ctrl Pts',(95.1416080119479,1.09021272333422E-14,
47.3866041859337));
#9407=CARTESIAN_POINT('Ctrl Pts',(92.0851458120341,1.05042416094065E-16,
49.0438828741821));
#9408=CARTESIAN_POINT('Ctrl Pts',(89.1070253835135,3.41156072033826E-15,
50.8477906894532));
#9409=CARTESIAN_POINT('Ctrl Pts',(86.1168527340107,1.03272048229725E-14,
52.6589987788881));
#9410=CARTESIAN_POINT('Ctrl Pts',(83.2056472832341,5.36384240903567E-14,
54.6180166790245));
#9411=CARTESIAN_POINT('Ctrl Pts',(80.3848301635821,3.08073424156598E-14,
56.721069668328));
#9412=CARTESIAN_POINT('Ctrl Pts',(77.5611534148135,1.32010255714472E-14,
58.8262546468059));
#9413=CARTESIAN_POINT('Ctrl Pts',(74.8381140101423,1.51039607992001E-14,
61.068519139977));
#9414=CARTESIAN_POINT('Ctrl Pts',(72.2297132774974,2.42097771138098E-14,
63.4364962704633));
#9415=CARTESIAN_POINT('Ctrl Pts',(69.6213194790238,1.66550167885819E-14,
65.8044671059204));
#9416=CARTESIAN_POINT('Ctrl Pts',(67.1275347240088,4.55894098149439E-14,
68.298071600504));
#9417=CARTESIAN_POINT('Ctrl Pts',(64.7594023581046,1.11217543556858E-14,
70.9062580231545));
#9418=CARTESIAN_POINT('Ctrl Pts',(62.4021012990924,-1.57438813545332E-14,
73.5025151854384));
#9419=CARTESIAN_POINT('Ctrl Pts',(60.1698465605612,-5.22446090150672E-14,
76.211731774115));
#9420=CARTESIAN_POINT('Ctrl Pts',(58.0726499521868,-2.90860017955518E-14,
79.0216408040366));
#9421=CARTESIAN_POINT('Ctrl Pts',(55.9948328500282,3.31444783804878E-15,
81.8055843859439));
#9422=CARTESIAN_POINT('Ctrl Pts',(54.0490749518631,-4.6343826823798E-14,
84.6891394721373));
#9423=CARTESIAN_POINT('Ctrl Pts',(52.2449416359332,-3.83898540398404E-14,
87.6582306461879));
#9424=CARTESIAN_POINT('Ctrl Pts',(50.4652489916249,-5.26518919980718E-14,
90.5870994144115));
#9425=CARTESIAN_POINT('Ctrl Pts',(48.8232383526351,1.12664867902641E-14,
93.5993053079775));
#9426=CARTESIAN_POINT('Ctrl Pts',(47.3258881353929,2.19975239907418E-14,
96.6820335276706));
#9427=CARTESIAN_POINT('Ctrl Pts',(45.8550866032248,3.66910777152371E-14,
99.7101036054466));
#9428=CARTESIAN_POINT('Ctrl Pts',(44.5237168473917,-5.11013660504775E-14,
102.806759783348));
#9429=CARTESIAN_POINT('Ctrl Pts',(43.3384647873199,-9.3811914345706E-14,
105.955904638828));
#9430=CARTESIAN_POINT('Ctrl Pts',(42.178411369753,-1.41776291118567E-13,
109.038098186581));
#9431=CARTESIAN_POINT('Ctrl Pts',(41.1578799651058,-8.19907887432609E-14,
112.171204882295));
#9432=CARTESIAN_POINT('Ctrl Pts',(40.2800279987793,-4.11497414918791E-14,
115.345683225176));
#9433=CARTESIAN_POINT('Ctrl Pts',(38.5944013814794,5.4727582458512E-14,
121.44122711647));
#9434=CARTESIAN_POINT('Ctrl Pts',(37.4373840532589,1.27133044339828E-13,
127.686816829449));
#9435=CARTESIAN_POINT('Ctrl Pts',(36.827675631427,-8.1444996146568E-14,
133.982075177761));
#9436=CARTESIAN_POINT('',(36.827675631427,-5.,133.982075177761));
#9437=CARTESIAN_POINT('',(145.859521458148,-5.,35.0000000000001));
#9438=CARTESIAN_POINT('Origin',(0.,-5.,130.415240784856));
#9439=CARTESIAN_POINT('Ctrl Pts',(-36.8276756314269,0.,133.982075177761));
#9440=CARTESIAN_POINT('Ctrl Pts',(-36.6797497079439,0.,135.50941492147));
#9441=CARTESIAN_POINT('Ctrl Pts',(-36.4288634825457,0.,137.114741394618));
#9442=CARTESIAN_POINT('Ctrl Pts',(-36.0405708212051,0.,138.786456639301));
#9443=CARTESIAN_POINT('Ctrl Pts',(-35.6522781598644,0.,140.458171883983));
#9444=CARTESIAN_POINT('Ctrl Pts',(-35.126304365244,0.,142.196602013066));
#9445=CARTESIAN_POINT('Ctrl Pts',(-34.4253505833173,0.,143.976038593824));
#9446=CARTESIAN_POINT('Ctrl Pts',(-33.7243968013906,0.,145.755475174581));
#9447=CARTESIAN_POINT('Ctrl Pts',(-32.8479279009936,0.,147.576162799206));
#9448=CARTESIAN_POINT('Ctrl Pts',(-31.7618111665595,0.,149.393843247098));
#9449=CARTESIAN_POINT('Ctrl Pts',(-30.6756944321254,0.,151.21152369499));
#9450=CARTESIAN_POINT('Ctrl Pts',(-29.3791356772816,0.,153.026147945389));
#9451=CARTESIAN_POINT('Ctrl Pts',(-27.8512109316029,0.,154.773197383129));
#9452=CARTESIAN_POINT('Ctrl Pts',(-26.3232861859242,0.,156.52024682087));
#9453=CARTESIAN_POINT('Ctrl Pts',(-24.5631346628349,0.,158.199131371192));
#9454=CARTESIAN_POINT('Ctrl Pts',(-22.5757614892594,0.,159.729656917198));
#9455=CARTESIAN_POINT('Ctrl Pts',(-20.5883883156839,0.,161.260182463203));
#9456=CARTESIAN_POINT('Ctrl Pts',(-18.3733019437227,0.,162.641132549651));
#9457=CARTESIAN_POINT('Ctrl Pts',(-15.972090553586,0.,163.790266228263));
#9458=CARTESIAN_POINT('Ctrl Pts',(-13.5708791634494,0.,164.939399906875));
#9459=CARTESIAN_POINT('Ctrl Pts',(-10.9839174320016,0.,165.855200551742));
#9460=CARTESIAN_POINT('Ctrl Pts',(-8.29064013714808,0.,166.474432208352));
#9461=CARTESIAN_POINT('Ctrl Pts',(-5.59736284229456,0.,167.093663864962));
#9462=CARTESIAN_POINT('Ctrl Pts',(-2.79913386299196,0.,167.415240784856));
#9463=CARTESIAN_POINT('Ctrl Pts',(1.41553435639707E-14,0.,167.415240784856));
#9464=CARTESIAN_POINT('Ctrl Pts',(2.79913386299198,0.,167.415240784856));
#9465=CARTESIAN_POINT('Ctrl Pts',(5.59736284229459,0.,167.093663864962));
#9466=CARTESIAN_POINT('Ctrl Pts',(8.29064013714809,0.,166.474432208352));
#9467=CARTESIAN_POINT('Ctrl Pts',(10.9839174320016,0.,165.855200551742));
#9468=CARTESIAN_POINT('Ctrl Pts',(13.5708791634494,0.,164.939399906875));
#9469=CARTESIAN_POINT('Ctrl Pts',(15.9720905535861,0.,163.790266228263));
#9470=CARTESIAN_POINT('Ctrl Pts',(18.3733019437227,0.,162.641132549651));
#9471=CARTESIAN_POINT('Ctrl Pts',(20.588388315684,0.,161.260182463203));
#9472=CARTESIAN_POINT('Ctrl Pts',(22.5757614892594,0.,159.729656917197));
#9473=CARTESIAN_POINT('Ctrl Pts',(24.5631346628349,0.,158.199131371192));
#9474=CARTESIAN_POINT('Ctrl Pts',(26.3232861859243,0.,156.52024682087));
#9475=CARTESIAN_POINT('Ctrl Pts',(27.851210931603,0.,154.773197383129));
#9476=CARTESIAN_POINT('Ctrl Pts',(29.3791356772816,0.,153.026147945389));
#9477=CARTESIAN_POINT('Ctrl Pts',(30.6756944321254,0.,151.21152369499));
#9478=CARTESIAN_POINT('Ctrl Pts',(31.7618111665595,0.,149.393843247098));
#9479=CARTESIAN_POINT('Ctrl Pts',(32.8479279009937,0.,147.576162799206));
#9480=CARTESIAN_POINT('Ctrl Pts',(33.7243968013906,0.,145.755475174581));
#9481=CARTESIAN_POINT('Ctrl Pts',(34.4253505833173,0.,143.976038593824));
#9482=CARTESIAN_POINT('Ctrl Pts',(35.126304365244,0.,142.196602013066));
#9483=CARTESIAN_POINT('Ctrl Pts',(35.6522781598644,0.,140.458171883983));
#9484=CARTESIAN_POINT('Ctrl Pts',(36.0405708212051,0.,138.786456639301));
#9485=CARTESIAN_POINT('Ctrl Pts',(36.4288634825457,0.,137.114741394618));
#9486=CARTESIAN_POINT('Ctrl Pts',(36.6797497079439,0.,135.50941492147));
#9487=CARTESIAN_POINT('Ctrl Pts',(36.8276756314269,0.,133.982075177761));
#9488=CARTESIAN_POINT('Ctrl Pts',(145.859521458148,3.17060992892912E-17,
35.0000000000001));
#9489=CARTESIAN_POINT('Ctrl Pts',(145.859521458148,3.17060992892912E-17,
35.0000000000001));
#9490=CARTESIAN_POINT('Ctrl Pts',(139.935495507955,1.0805348367736,35.0000000000001));
#9491=CARTESIAN_POINT('Ctrl Pts',(139.721849114783,-0.00946396649206172,
35.0000000000001));
#9492=CARTESIAN_POINT('Ctrl Pts',(134.282043748658,2.43566561952011,35.0000000000001));
#9493=CARTESIAN_POINT('Ctrl Pts',(133.377109515712,-0.02133300752971,35.5229040509096));
#9494=CARTESIAN_POINT('Ctrl Pts',(126.153138109028,4.82540450931202,35.0000000000001));
#9495=CARTESIAN_POINT('Ctrl Pts',(123.752347112548,-0.0422637614564399,
37.2196520098122));
#9496=CARTESIAN_POINT('Ctrl Pts',(123.502048229037,5.68149125852134,35.0000000000001));
#9497=CARTESIAN_POINT('Ctrl Pts',(120.526890370995,-0.0497618781603927,
37.9367613539355));
#9498=CARTESIAN_POINT('Ctrl Pts',(118.307860920989,7.50353712828282,35.0000000000001));
#9499=CARTESIAN_POINT('Ctrl Pts',(114.083064301351,-0.0657204391170305,
39.6868647729585));
#9500=CARTESIAN_POINT('Ctrl Pts',(115.764763492932,8.46949624883498,35.0000000000001));
#9501=CARTESIAN_POINT('Ctrl Pts',(110.864745388532,-0.0741808833697154,
40.7198997814395));
#9502=CARTESIAN_POINT('Ctrl Pts',(110.777462874248,10.5021449940676,35.0000000000001));
#9503=CARTESIAN_POINT('Ctrl Pts',(104.480363407898,-0.091984029515797,43.1072738736836));
#9504=CARTESIAN_POINT('Ctrl Pts',(108.33325968362,11.568834618748,35.0000000000001));
#9505=CARTESIAN_POINT('Ctrl Pts',(101.314363685346,-0.101326731409194,44.4616401695737));
#9506=CARTESIAN_POINT('Ctrl Pts',(103.53464932529,13.7938025050227,35.0000000000001));
#9507=CARTESIAN_POINT('Ctrl Pts',(95.0816761504739,-0.120814322928678,47.488542779257));
#9508=CARTESIAN_POINT('Ctrl Pts',(101.180242157587,14.9520807666169,35.0000000000001));
#9509=CARTESIAN_POINT('Ctrl Pts',(92.0150600641061,-0.130959212554766,49.1610880733554));
#9510=CARTESIAN_POINT('Ctrl Pts',(96.5521256306011,17.3510840595046,35.0000000000001));
#9511=CARTESIAN_POINT('Ctrl Pts',(86.0280376785636,-0.151971109631613,52.8121020506907));
#9512=CARTESIAN_POINT('Ctrl Pts',(94.2784162713182,18.591809090798,35.0000000000001));
#9513=CARTESIAN_POINT('Ctrl Pts',(83.1077052252586,-0.162838117082372,54.790558780279));
#9514=CARTESIAN_POINT('Ctrl Pts',(89.8025971466679,21.1465640558695,35.0000000000001));
#9515=CARTESIAN_POINT('Ctrl Pts',(77.4577804126425,-0.18521417990054,59.0320726395877));
#9516=CARTESIAN_POINT('Ctrl Pts',(87.6004873813004,22.4605939896476,35.0000000000001));
#9517=CARTESIAN_POINT('Ctrl Pts',(74.7282568878096,-0.19672323526795,61.2950966764346));
#9518=CARTESIAN_POINT('Ctrl Pts',(83.2587692299763,25.1528168924739,35.0000000000001));
#9519=CARTESIAN_POINT('Ctrl Pts',(69.4999442605203,-0.220303324011399,66.0760233448773));
#9520=CARTESIAN_POINT('Ctrl Pts',(81.1191608440196,26.5310098615222,35.0000000000001));
#9521=CARTESIAN_POINT('Ctrl Pts',(67.0012121018892,-0.232374357387438,68.5938742813195));
#9522=CARTESIAN_POINT('Ctrl Pts',(76.8933472370124,29.3424169676742,35.0000000000001));
#9523=CARTESIAN_POINT('Ctrl Pts',(62.2680278203847,-0.256998332240127,73.8476184739701));
#9524=CARTESIAN_POINT('Ctrl Pts',(74.8071420159619,30.7756311047781,35.0000000000001));
#9525=CARTESIAN_POINT('Ctrl Pts',(60.0336152719651,-0.269551273716776,76.583446406475));
#9526=CARTESIAN_POINT('Ctrl Pts',(70.6790365242624,33.6879386798268,35.0000000000001));
#9527=CARTESIAN_POINT('Ctrl Pts',(55.8546997737931,-0.295058994862664,82.2309706047639));
#9528=CARTESIAN_POINT('Ctrl Pts',(68.6371362536135,35.1670321177717,35.0000000000001));
#9529=CARTESIAN_POINT('Ctrl Pts',(53.9102158408265,-0.308013774531903,85.1425945209522));
#9530=CARTESIAN_POINT('Ctrl Pts',(64.5885424482125,38.1619564272879,35.0000000000001));
#9531=CARTESIAN_POINT('Ctrl Pts',(50.3279822508715,-0.334245102154949,91.0962909513875));
#9532=CARTESIAN_POINT('Ctrl Pts',(62.5818489134604,39.6777872988593,35.0000000000001));
#9533=CARTESIAN_POINT('Ctrl Pts',(48.6902305698515,-0.347521650108757,94.1382912080291));
#9534=CARTESIAN_POINT('Ctrl Pts',(58.5945703653485,42.7370446084141,35.0000000000001));
#9535=CARTESIAN_POINT('Ctrl Pts',(45.729227108235,-0.374316444392921,100.306271688078));
#9536=CARTESIAN_POINT('Ctrl Pts',(56.6139853519887,44.2804710463974,35.0000000000001));
#9537=CARTESIAN_POINT('Ctrl Pts',(44.4059543487921,-0.387834690723277,103.432186237973));
#9538=CARTESIAN_POINT('Ctrl Pts',(52.6698256321568,47.3857776215616,35.0000000000001));
#9539=CARTESIAN_POINT('Ctrl Pts',(42.0729707183869,-0.415032811852518,109.722571033699));
#9540=CARTESIAN_POINT('Ctrl Pts',(50.7062509256847,48.9476577587424,35.0000000000001));
#9541=CARTESIAN_POINT('Ctrl Pts',(41.063223964567,-0.428712686651402,112.886987153028));
#9542=CARTESIAN_POINT('Ctrl Pts',(44.8273949448428,53.6472659182591,35.0000000000001));
#9543=CARTESIAN_POINT('Ctrl Pts',(38.4911694061933,-0.469874648888817,122.374221150099));
#9544=CARTESIAN_POINT('Ctrl Pts',(40.9239818090477,56.7989616885694,35.0000000000001));
#9545=CARTESIAN_POINT('Ctrl Pts',(37.3884769379574,-0.497479074168109,128.688287898515));
#9546=CARTESIAN_POINT('Ctrl Pts',(37.,59.9327136539873,35.0000000000001));
#9547=CARTESIAN_POINT('Ctrl Pts',(36.826166312158,-0.524926336936336,134.849019038261));
#9548=CARTESIAN_POINT('',(37.,59.9327136539873,35.0000000000001));
#9549=CARTESIAN_POINT('Ctrl Pts',(37.,59.9327136539873,35.0000000000001));
#9550=CARTESIAN_POINT('Ctrl Pts',(63.6931530394734,38.6151528519019,35.0000000000001));
#9551=CARTESIAN_POINT('Ctrl Pts',(89.4344921386865,16.4672437124081,35.0000000000001));
#9552=CARTESIAN_POINT('Ctrl Pts',(125.680065601263,5.0000000000004,35.0000000000001));
#9553=CARTESIAN_POINT('',(37.,59.9327136539873,35.0000000000001));
#9554=CARTESIAN_POINT('Ctrl Pts',(145.859521458148,3.17060992892912E-17,
35.0000000000001));
#9555=CARTESIAN_POINT('Ctrl Pts',(139.935495507955,1.0805348367736,35.0000000000001));
#9556=CARTESIAN_POINT('Ctrl Pts',(134.282043748658,2.43566561952011,35.0000000000001));
#9557=CARTESIAN_POINT('Ctrl Pts',(127.792835858035,4.34336551759297,35.0000000000001));
#9558=CARTESIAN_POINT('Ctrl Pts',(126.732026641535,4.66718436287958,35.0000000000001));
#9559=CARTESIAN_POINT('Ctrl Pts',(125.680065601264,5.,35.0000000000001));
#9560=CARTESIAN_POINT('Ctrl Pts',(-37.,59.9327136539873,35.0000000000001));
#9561=CARTESIAN_POINT('Ctrl Pts',(-36.8261663120238,-0.524926383580335,
134.849019115296));
#9562=CARTESIAN_POINT('Ctrl Pts',(-40.9239818090476,56.7989616885694,35.0000000000001));
#9563=CARTESIAN_POINT('Ctrl Pts',(-37.3884769352297,-0.497479118373195,
128.688287970797));
#9564=CARTESIAN_POINT('Ctrl Pts',(-44.8273949448428,53.6472659182591,35.0000000000001));
#9565=CARTESIAN_POINT('Ctrl Pts',(-38.4911694013047,-0.469874690641024,
122.374221217509));
#9566=CARTESIAN_POINT('Ctrl Pts',(-50.7062509256847,48.9476577587424,35.0000000000001));
#9567=CARTESIAN_POINT('Ctrl Pts',(-41.0632239571272,-0.428712724746032,
112.886987213119));
#9568=CARTESIAN_POINT('Ctrl Pts',(-52.6698256321568,47.3857776215616,35.0000000000001));
#9569=CARTESIAN_POINT('Ctrl Pts',(-42.0729707102112,-0.415032848731579,
109.722571091349));
#9570=CARTESIAN_POINT('Ctrl Pts',(-56.6139853519887,44.2804710463974,35.0000000000001));
#9571=CARTESIAN_POINT('Ctrl Pts',(-44.4059543393734,-0.387834725185562,
103.432186290769));
#9572=CARTESIAN_POINT('Ctrl Pts',(-58.5945703653485,42.7370446084141,35.0000000000001));
#9573=CARTESIAN_POINT('Ctrl Pts',(-45.7292270983091,-0.374316477654,100.306271738463));
#9574=CARTESIAN_POINT('Ctrl Pts',(-62.5818489134604,39.6777872988593,35.0000000000001));
#9575=CARTESIAN_POINT('Ctrl Pts',(-48.6902305591338,-0.347521680988899,
94.1382912536552));
#9576=CARTESIAN_POINT('Ctrl Pts',(-64.5885424482124,38.1619564272879,35.0000000000001));
#9577=CARTESIAN_POINT('Ctrl Pts',(-50.3279822398692,-0.334245131855361,
91.0962909946666));
#9578=CARTESIAN_POINT('Ctrl Pts',(-68.6371362536135,35.1670321177717,35.0000000000001));
#9579=CARTESIAN_POINT('Ctrl Pts',(-53.9102158294643,-0.308013801901447,
85.1425945596379));
#9580=CARTESIAN_POINT('Ctrl Pts',(-70.6790365242624,33.6879386798268,35.0000000000001));
#9581=CARTESIAN_POINT('Ctrl Pts',(-55.8546997623558,-0.29505902108107,82.2309706412034));
#9582=CARTESIAN_POINT('Ctrl Pts',(-74.8071420159619,30.7756311047781,35.0000000000001));
#9583=CARTESIAN_POINT('Ctrl Pts',(-60.033615260567,-0.269551297668613,76.5834464385573));
#9584=CARTESIAN_POINT('Ctrl Pts',(-76.8933472370124,29.3424169676743,35.0000000000001));
#9585=CARTESIAN_POINT('Ctrl Pts',(-62.2680278091009,-0.256998355076532,
73.8476185039417));
#9586=CARTESIAN_POINT('Ctrl Pts',(-81.1191608440196,26.5310098615222,35.0000000000001));
#9587=CARTESIAN_POINT('Ctrl Pts',(-67.0012120909969,-0.232374378035801,
68.5938743072377));
#9588=CARTESIAN_POINT('Ctrl Pts',(-83.2587692299763,25.152816892474,35.0000000000001));
#9589=CARTESIAN_POINT('Ctrl Pts',(-69.499944249905,-0.220303343587152,66.0760233688529));
#9590=CARTESIAN_POINT('Ctrl Pts',(-87.6004873813004,22.4605939896476,35.0000000000001));
#9591=CARTESIAN_POINT('Ctrl Pts',(-74.7282568778784,-0.196723252748419,
61.2950966967217));
#9592=CARTESIAN_POINT('Ctrl Pts',(-89.8025971466678,21.1465640558695,35.0000000000001));
#9593=CARTESIAN_POINT('Ctrl Pts',(-77.4577804031182,-0.185214196358336,
59.0320726581288));
#9594=CARTESIAN_POINT('Ctrl Pts',(-94.2784162713182,18.591809090798,35.0000000000001));
#9595=CARTESIAN_POINT('Ctrl Pts',(-83.1077052166401,-0.162838131551871,
54.7905587955477));
#9596=CARTESIAN_POINT('Ctrl Pts',(-96.5521256306011,17.3510840595046,35.0000000000001));
#9597=CARTESIAN_POINT('Ctrl Pts',(-86.0280376704441,-0.15197112313549,52.812102064433));
#9598=CARTESIAN_POINT('Ctrl Pts',(-101.180242157587,14.9520807666169,35.0000000000001));
#9599=CARTESIAN_POINT('Ctrl Pts',(-92.0150600570349,-0.130959224191564,
49.1610880842809));
#9600=CARTESIAN_POINT('Ctrl Pts',(-103.53464932529,13.7938025050227,35.0000000000001));
#9601=CARTESIAN_POINT('Ctrl Pts',(-95.0816761439523,-0.120814333664019,
47.4885427888921));
#9602=CARTESIAN_POINT('Ctrl Pts',(-108.33325968362,11.568834618748,35.0000000000001));
#9603=CARTESIAN_POINT('Ctrl Pts',(-101.314363679931,-0.101326740412903,
44.4616401768735));
#9604=CARTESIAN_POINT('Ctrl Pts',(-110.777462874248,10.5021449940676,35.0000000000001));
#9605=CARTESIAN_POINT('Ctrl Pts',(-104.48036340304,-0.0919840376893306,
43.1072738799385));
#9606=CARTESIAN_POINT('Ctrl Pts',(-115.764763492932,8.46949624883498,35.0000000000001));
#9607=CARTESIAN_POINT('Ctrl Pts',(-110.864745384751,-0.0741808899612938,
40.7198997858525));
#9608=CARTESIAN_POINT('Ctrl Pts',(-118.307860920989,7.50353712828282,35.0000000000001));
#9609=CARTESIAN_POINT('Ctrl Pts',(-114.083064298091,-0.0657204449568292,
39.6868647765745));
#9610=CARTESIAN_POINT('Ctrl Pts',(-123.502048229037,5.68149125852133,35.0000000000001));
#9611=CARTESIAN_POINT('Ctrl Pts',(-120.5268903687,-0.0497618825821426,37.9367613562013));
#9612=CARTESIAN_POINT('Ctrl Pts',(-126.153138109028,4.82540450931201,35.0000000000001));
#9613=CARTESIAN_POINT('Ctrl Pts',(-123.752347110696,-0.0422637652119208,
37.2196520115247));
#9614=CARTESIAN_POINT('Ctrl Pts',(-134.282043748658,2.43566561952011,35.0000000000001));
#9615=CARTESIAN_POINT('Ctrl Pts',(-133.377109515013,-0.0213330094253222,
35.5229040513131));
#9616=CARTESIAN_POINT('Ctrl Pts',(-139.935495507955,1.08053483677359,35.0000000000001));
#9617=CARTESIAN_POINT('Ctrl Pts',(-139.721849114618,-0.00946396733301255,
35.0000000000001));
#9618=CARTESIAN_POINT('Ctrl Pts',(-145.859521458148,3.17060992892922E-17,
35.0000000000001));
#9619=CARTESIAN_POINT('Ctrl Pts',(-145.859521458148,3.17060992892922E-17,
35.0000000000001));
#9620=CARTESIAN_POINT('Ctrl Pts',(-145.859521458148,0.,35.0000000000001));
#9621=CARTESIAN_POINT('Ctrl Pts',(-138.765903145092,1.29386700370264,35.0000000000001));
#9622=CARTESIAN_POINT('Ctrl Pts',(-132.060245856224,2.98146159866235,35.0000000000001));
#9623=CARTESIAN_POINT('Ctrl Pts',(-125.680065601258,5.00000000000191,35.0000000000001));
#9624=CARTESIAN_POINT('',(-37.,59.9327136539873,35.0000000000001));
#9625=CARTESIAN_POINT('',(-36.8276756314269,0.,133.982075177761));
#9626=CARTESIAN_POINT('Ctrl Pts',(-125.680065601258,5.00000000000191,35.0000000000001));
#9627=CARTESIAN_POINT('Ctrl Pts',(-89.4344921386844,16.4672437124101,35.0000000000001));
#9628=CARTESIAN_POINT('Ctrl Pts',(-63.6931530394722,38.6151528519028,35.0000000000001));
#9629=CARTESIAN_POINT('Ctrl Pts',(-37.,59.9327136539873,35.0000000000001));
#9630=CARTESIAN_POINT('Ctrl Pts',(37.,59.9327136539873,35.0000000000001));
#9631=CARTESIAN_POINT('Ctrl Pts',(36.8276756314269,0.,133.982075177761));
#9632=CARTESIAN_POINT('Ctrl Pts',(35.9620587845551,61.072632135455,35.0000000000001));
#9633=CARTESIAN_POINT('Ctrl Pts',(36.6797497079439,0.,135.50941492147));
#9634=CARTESIAN_POINT('Ctrl Pts',(34.8494287906845,62.1881303927957,35.0000000000001));
#9635=CARTESIAN_POINT('Ctrl Pts',(36.4288634825457,0.,137.114741394618));
#9636=CARTESIAN_POINT('Ctrl Pts',(32.4772932645476,64.3449801372208,35.0000000000001));
#9637=CARTESIAN_POINT('Ctrl Pts',(35.6522781598644,0.,140.458171883983));
#9638=CARTESIAN_POINT('Ctrl Pts',(31.2177877322813,65.3863316243053,35.0000000000001));
#9639=CARTESIAN_POINT('Ctrl Pts',(35.126304365244,0.,142.196602013066));
#9640=CARTESIAN_POINT('Ctrl Pts',(28.5544031478084,67.3695815062162,35.0000000000001));
#9641=CARTESIAN_POINT('Ctrl Pts',(33.7243968013906,0.,145.755475174581));
#9642=CARTESIAN_POINT('Ctrl Pts',(27.1503938737515,68.3111074622806,35.0000000000001));
#9643=CARTESIAN_POINT('Ctrl Pts',(32.8479279009937,0.,147.576162799206));
#9644=CARTESIAN_POINT('Ctrl Pts',(24.2115292157522,70.0684707648054,35.0000000000001));
#9645=CARTESIAN_POINT('Ctrl Pts',(30.6756944321254,0.,151.21152369499));
#9646=CARTESIAN_POINT('Ctrl Pts',(22.6766738318099,70.8843081112658,35.0000000000001));
#9647=CARTESIAN_POINT('Ctrl Pts',(29.3791356772816,0.,153.026147945389));
#9648=CARTESIAN_POINT('Ctrl Pts',(19.4899048077957,72.3648035547606,35.0000000000001));
#9649=CARTESIAN_POINT('Ctrl Pts',(26.3232861859243,0.,156.52024682087));
#9650=CARTESIAN_POINT('Ctrl Pts',(17.8381180298111,73.0290133496626,35.0000000000001));
#9651=CARTESIAN_POINT('Ctrl Pts',(24.5631346628349,0.,158.199131371192));
#9652=CARTESIAN_POINT('Ctrl Pts',(14.4429405853757,74.1860012886773,35.0000000000001));
#9653=CARTESIAN_POINT('Ctrl Pts',(20.588388315684,0.,161.260182463203));
#9654=CARTESIAN_POINT('Ctrl Pts',(12.6995499189249,74.6787794327899,35.0000000000001));
#9655=CARTESIAN_POINT('Ctrl Pts',(18.3733019437227,0.,162.641132549651));
#9656=CARTESIAN_POINT('Ctrl Pts',(9.14636534104553,75.4735482731269,35.0000000000001));
#9657=CARTESIAN_POINT('Ctrl Pts',(13.5708791634494,0.,164.939399906875));
#9658=CARTESIAN_POINT('Ctrl Pts',(7.33698151150071,75.775223998754,35.0000000000001));
#9659=CARTESIAN_POINT('Ctrl Pts',(10.9839174320016,0.,165.855200551742));
#9660=CARTESIAN_POINT('Ctrl Pts',(3.68515441892942,76.1798832399239,35.0000000000001));
#9661=CARTESIAN_POINT('Ctrl Pts',(5.59736284229459,0.,167.093663864962));
#9662=CARTESIAN_POINT('Ctrl Pts',(1.84271115590295,76.2828667554667,35.0000000000001));
#9663=CARTESIAN_POINT('Ctrl Pts',(2.79913386299198,0.,167.415240784856));
#9664=CARTESIAN_POINT('Ctrl Pts',(-1.84271115590294,76.2828667554667,35.0000000000001));
#9665=CARTESIAN_POINT('Ctrl Pts',(-2.79913386299196,0.,167.415240784856));
#9666=CARTESIAN_POINT('Ctrl Pts',(-3.68515441892941,76.1798832399239,35.0000000000001));
#9667=CARTESIAN_POINT('Ctrl Pts',(-5.59736284229456,0.,167.093663864962));
#9668=CARTESIAN_POINT('Ctrl Pts',(-7.3369815115007,75.775223998754,35.0000000000001));
#9669=CARTESIAN_POINT('Ctrl Pts',(-10.9839174320016,0.,165.855200551742));
#9670=CARTESIAN_POINT('Ctrl Pts',(-9.14636534104552,75.4735482731269,35.0000000000001));
#9671=CARTESIAN_POINT('Ctrl Pts',(-13.5708791634494,0.,164.939399906875));
#9672=CARTESIAN_POINT('Ctrl Pts',(-12.6995499189248,74.6787794327899,35.0000000000001));
#9673=CARTESIAN_POINT('Ctrl Pts',(-18.3733019437227,0.,162.641132549651));
#9674=CARTESIAN_POINT('Ctrl Pts',(-14.4429405853757,74.1860012886772,35.0000000000001));
#9675=CARTESIAN_POINT('Ctrl Pts',(-20.5883883156839,0.,161.260182463203));
#9676=CARTESIAN_POINT('Ctrl Pts',(-17.8381180298111,73.0290133496626,35.0000000000001));
#9677=CARTESIAN_POINT('Ctrl Pts',(-24.5631346628349,0.,158.199131371192));
#9678=CARTESIAN_POINT('Ctrl Pts',(-19.4899048077957,72.3648035547606,35.0000000000001));
#9679=CARTESIAN_POINT('Ctrl Pts',(-26.3232861859242,0.,156.52024682087));
#9680=CARTESIAN_POINT('Ctrl Pts',(-22.6766738318099,70.8843081112658,35.0000000000001));
#9681=CARTESIAN_POINT('Ctrl Pts',(-29.3791356772816,0.,153.026147945389));
#9682=CARTESIAN_POINT('Ctrl Pts',(-24.2115292157522,70.0684707648055,35.0000000000001));
#9683=CARTESIAN_POINT('Ctrl Pts',(-30.6756944321254,0.,151.21152369499));
#9684=CARTESIAN_POINT('Ctrl Pts',(-27.1503938737515,68.3111074622806,35.0000000000001));
#9685=CARTESIAN_POINT('Ctrl Pts',(-32.8479279009936,0.,147.576162799206));
#9686=CARTESIAN_POINT('Ctrl Pts',(-28.5544031478084,67.3695815062162,35.0000000000001));
#9687=CARTESIAN_POINT('Ctrl Pts',(-33.7243968013906,0.,145.755475174581));
#9688=CARTESIAN_POINT('Ctrl Pts',(-31.2177877322813,65.3863316243053,35.0000000000001));
#9689=CARTESIAN_POINT('Ctrl Pts',(-35.126304365244,0.,142.196602013066));
#9690=CARTESIAN_POINT('Ctrl Pts',(-32.4772932645476,64.3449801372208,35.0000000000001));
#9691=CARTESIAN_POINT('Ctrl Pts',(-35.6522781598644,0.,140.458171883983));
#9692=CARTESIAN_POINT('Ctrl Pts',(-34.8494287906845,62.1881303927957,35.0000000000001));
#9693=CARTESIAN_POINT('Ctrl Pts',(-36.4288634825457,0.,137.114741394618));
#9694=CARTESIAN_POINT('Ctrl Pts',(-35.9620587845551,61.0726321354551,35.0000000000001));
#9695=CARTESIAN_POINT('Ctrl Pts',(-36.6797497079439,0.,135.50941492147));
#9696=CARTESIAN_POINT('Ctrl Pts',(-37.,59.9327136539873,35.0000000000001));
#9697=CARTESIAN_POINT('Ctrl Pts',(-36.8276756314269,0.,133.982075177761));
#9698=CARTESIAN_POINT('Ctrl Pts',(-37.,59.9327136539873,35.0000000000001));
#9699=CARTESIAN_POINT('Ctrl Pts',(-34.9241175691101,62.2125506169229,35.0000000000001));
#9700=CARTESIAN_POINT('Ctrl Pts',(-32.5494800245177,64.3947066833499,35.0000000000001));
#9701=CARTESIAN_POINT('Ctrl Pts',(-29.8860954400449,66.3779565652608,35.0000000000001));
#9702=CARTESIAN_POINT('Ctrl Pts',(-27.222710855572,68.3612064471716,35.0000000000001));
#9703=CARTESIAN_POINT('Ctrl Pts',(-24.270058343817,70.1440603895185,35.0000000000001));
#9704=CARTESIAN_POINT('Ctrl Pts',(-21.0832893198028,71.6245558330132,35.0000000000001));
#9705=CARTESIAN_POINT('Ctrl Pts',(-17.8965202957886,73.105051276508,35.0000000000001));
#9706=CARTESIAN_POINT('Ctrl Pts',(-14.4761422078645,74.2813950126213,35.0000000000001));
#9707=CARTESIAN_POINT('Ctrl Pts',(-10.9229576299852,75.0761638529584,35.0000000000001));
#9708=CARTESIAN_POINT('Ctrl Pts',(-7.36977305210586,75.8709326932955,35.0000000000001));
#9709=CARTESIAN_POINT('Ctrl Pts',(-3.68542231180589,76.2828667554667,35.0000000000001));
#9710=CARTESIAN_POINT('Ctrl Pts',(8.60422844084496E-15,76.2828667554667,
35.0000000000001));
#9711=CARTESIAN_POINT('Ctrl Pts',(3.68542231180591,76.2828667554667,35.0000000000001));
#9712=CARTESIAN_POINT('Ctrl Pts',(7.36977305210588,75.8709326932955,35.0000000000001));
#9713=CARTESIAN_POINT('Ctrl Pts',(10.9229576299852,75.0761638529584,35.0000000000001));
#9714=CARTESIAN_POINT('Ctrl Pts',(14.4761422078645,74.2813950126214,35.0000000000001));
#9715=CARTESIAN_POINT('Ctrl Pts',(17.8965202957886,73.105051276508,35.0000000000001));
#9716=CARTESIAN_POINT('Ctrl Pts',(21.0832893198028,71.6245558330132,35.0000000000001));
#9717=CARTESIAN_POINT('Ctrl Pts',(24.2700583438171,70.1440603895185,35.0000000000001));
#9718=CARTESIAN_POINT('Ctrl Pts',(27.222710855572,68.3612064471716,35.0000000000001));
#9719=CARTESIAN_POINT('Ctrl Pts',(29.8860954400449,66.3779565652607,35.0000000000001));
#9720=CARTESIAN_POINT('Ctrl Pts',(32.5494800245177,64.3947066833499,35.0000000000001));
#9721=CARTESIAN_POINT('Ctrl Pts',(34.9241175691101,62.2125506169228,35.0000000000001));
#9722=CARTESIAN_POINT('Ctrl Pts',(37.,59.9327136539873,35.0000000000001));
#9723=CARTESIAN_POINT('Ctrl Pts',(-126.333741430004,4.79470864688834,25.0000000000001));
#9724=CARTESIAN_POINT('Ctrl Pts',(-126.333741430004,4.79470864688834,37.0000000000001));
#9725=CARTESIAN_POINT('Ctrl Pts',(-89.7434098754838,16.201390763878,25.0000000000001));
#9726=CARTESIAN_POINT('Ctrl Pts',(-89.7434098754838,16.201390763878,37.0000000000001));
#9727=CARTESIAN_POINT('Ctrl Pts',(-63.8533409646905,38.4872243216708,25.0000000000001));
#9728=CARTESIAN_POINT('Ctrl Pts',(-63.8533409646905,38.4872243216708,37.0000000000001));
#9729=CARTESIAN_POINT('Ctrl Pts',(-37.,59.9327136539873,25.0000000000001));
#9730=CARTESIAN_POINT('Ctrl Pts',(-37.,59.9327136539873,37.0000000000001));
#9731=CARTESIAN_POINT('',(-37.,59.9327136539873,25.0000000000001));
#9732=CARTESIAN_POINT('Origin',(5.94655548926424E-16,26.2427388041954,25.0000000000001));
#9733=CARTESIAN_POINT('',(20.,72.1122755947453,-11.9999999999999));
#9734=CARTESIAN_POINT('Ctrl Pts',(-20.,72.1122755947453,-11.9999999999999));
#9735=CARTESIAN_POINT('Ctrl Pts',(-20.,72.1122755947453,-10.7281705881235));
#9736=CARTESIAN_POINT('Ctrl Pts',(-19.876740954423,72.1666695578122,-9.41819722511157));
#9737=CARTESIAN_POINT('Ctrl Pts',(-19.363419845374,72.3854545732174,-6.82230663106049));
#9738=CARTESIAN_POINT('Ctrl Pts',(-18.9735260730669,72.5495796554118,-5.53633371502868));
#9739=CARTESIAN_POINT('Ctrl Pts',(-17.9489707104667,72.9562551485406,-3.07765863937579));
#9740=CARTESIAN_POINT('Ctrl Pts',(-17.3134969066183,73.1986589652098,-1.90272848601112));
#9741=CARTESIAN_POINT('Ctrl Pts',(-15.8503625531969,73.7125357294074,0.266950487449766));
#9742=CARTESIAN_POINT('Ctrl Pts',(-15.0225516277294,73.9834946181185,1.26171961973252));
#9743=CARTESIAN_POINT('Ctrl Pts',(-13.2626071807075,74.5020216025358,3.02166406675442));
#9744=CARTESIAN_POINT('Ctrl Pts',(-12.2682645673177,74.7684339328333,3.84936166480408));
#9745=CARTESIAN_POINT('Ctrl Pts',(-10.0983665793023,75.2659618277825,5.31287304805954));
#9746=CARTESIAN_POINT('Ctrl Pts',(-8.92278917997,75.4966497262723,5.94879953171039));
#9747=CARTESIAN_POINT('Ctrl Pts',(-6.46280366693619,75.8793792723685,6.97387010022773));
#9748=CARTESIAN_POINT('Ctrl Pts',(-5.17618585589729,76.0314587231336,7.36382898538741));
#9749=CARTESIAN_POINT('Ctrl Pts',(-2.58007773937013,76.2332652071209,7.87697089230036));
#9750=CARTESIAN_POINT('Ctrl Pts',(-1.2705472609979,76.2828667554667,8.00000000000007));
#9751=CARTESIAN_POINT('Ctrl Pts',(1.2705472609979,76.2828667554667,8.00000000000007));
#9752=CARTESIAN_POINT('Ctrl Pts',(2.58007773937013,76.2332652071209,7.87697089230036));
#9753=CARTESIAN_POINT('Ctrl Pts',(5.17618585589729,76.0314587231336,7.36382898538741));
#9754=CARTESIAN_POINT('Ctrl Pts',(6.46280366693619,75.8793792723685,6.97387010022773));
#9755=CARTESIAN_POINT('Ctrl Pts',(8.92278917997,75.4966497262723,5.94879953171039));
#9756=CARTESIAN_POINT('Ctrl Pts',(10.0983665793023,75.2659618277825,5.31287304805954));
#9757=CARTESIAN_POINT('Ctrl Pts',(12.2682645673177,74.7684339328333,3.84936166480408));
#9758=CARTESIAN_POINT('Ctrl Pts',(13.2626071807075,74.5020216025358,3.02166406675442));
#9759=CARTESIAN_POINT('Ctrl Pts',(15.0225516277294,73.9834946181185,1.26171961973252));
#9760=CARTESIAN_POINT('Ctrl Pts',(15.8503625531969,73.7125357294074,0.266950487449763));
#9761=CARTESIAN_POINT('Ctrl Pts',(17.3134969066183,73.1986589652098,-1.90272848601112));
#9762=CARTESIAN_POINT('Ctrl Pts',(17.9489707104667,72.9562551485406,-3.07765863937579));
#9763=CARTESIAN_POINT('Ctrl Pts',(18.9735260730669,72.5495796554118,-5.53633371502868));
#9764=CARTESIAN_POINT('Ctrl Pts',(19.363419845374,72.3854545732174,-6.82230663106049));
#9765=CARTESIAN_POINT('Ctrl Pts',(19.876740954423,72.1666695578122,-9.41819722511157));
#9766=CARTESIAN_POINT('Ctrl Pts',(20.,72.1122755947453,-10.7281705881235));
#9767=CARTESIAN_POINT('Ctrl Pts',(20.,72.1122755947453,-11.9999999999999));
#9768=CARTESIAN_POINT('',(-20.,72.1122755947453,-11.9999999999999));
#9769=CARTESIAN_POINT('',(37.,59.9327136539873,25.0000000000001));
#9770=CARTESIAN_POINT('Ctrl Pts',(37.,59.9327136539873,25.0000000000001));
#9771=CARTESIAN_POINT('Ctrl Pts',(37.,59.9327136539873,37.0000000000001));
#9772=CARTESIAN_POINT('Ctrl Pts',(63.8533446476634,38.4872213803922,25.0000000000001));
#9773=CARTESIAN_POINT('Ctrl Pts',(63.8533446476634,38.4872213803922,37.0000000000001));
#9774=CARTESIAN_POINT('Ctrl Pts',(89.7434169772014,16.2013846508122,25.0000000000001));
#9775=CARTESIAN_POINT('Ctrl Pts',(89.7434169772014,16.2013846508122,37.0000000000001));
#9776=CARTESIAN_POINT('Ctrl Pts',(126.333756485248,4.79470395356222,25.0000000000001));
#9777=CARTESIAN_POINT('Ctrl Pts',(126.333756485248,4.79470395356222,37.0000000000001));
#9778=CARTESIAN_POINT('Origin',(37.,-5.,35.0000000000001));
#9779=CARTESIAN_POINT('',(-145.859521458148,0.,35.0000000000001));
#9780=CARTESIAN_POINT('Origin',(37.,-5.,35.0000000000001));
#9781=CARTESIAN_POINT('',(145.859521458148,0.,35.0000000000001));
#9782=CARTESIAN_POINT('Origin',(-99.7519848385422,-5.,-11.9999999999999));
#9783=CARTESIAN_POINT('',(-145.859521458148,-5.,-58.9999999999999));
#9784=CARTESIAN_POINT('Origin',(99.7519848385422,-5.,-11.9999999999999));
#9785=CARTESIAN_POINT('',(145.859521458148,-5.,-59.));
#9786=CARTESIAN_POINT('Origin',(-145.859521458148,-4.99999999999993,-168.542028553823));
#9787=CARTESIAN_POINT('',(-36.827675631427,6.20110919257889E-14,-157.982075177761));
#9788=CARTESIAN_POINT('Ctrl Pts',(-145.859521458148,1.99232991215936E-14,
-58.9999999999999));
#9789=CARTESIAN_POINT('Ctrl Pts',(-145.635702363347,0.000231282966572025,
-58.9999999999999));
#9790=CARTESIAN_POINT('Ctrl Pts',(-145.411883254566,0.000447783515656521,
-59.0006859694108));
#9791=CARTESIAN_POINT('Ctrl Pts',(-145.18806728541,0.000650024995078429,
-59.0020579084895));
#9792=CARTESIAN_POINT('Ctrl Pts',(-139.052999251965,0.00619371001492337,
-59.039664427889));
#9793=CARTESIAN_POINT('Ctrl Pts',(-132.962545443942,9.41456194013237E-14,
-59.592285658951));
#9794=CARTESIAN_POINT('Ctrl Pts',(-126.977116946521,7.40439610666388E-14,
-60.6397078209218));
#9795=CARTESIAN_POINT('Ctrl Pts',(-123.729336577931,6.46076837229338E-14,
-61.208054287134));
#9796=CARTESIAN_POINT('Ctrl Pts',(-120.512481495564,9.59966811121834E-14,
-61.9221153240676));
#9797=CARTESIAN_POINT('Ctrl Pts',(-117.336234309904,9.53981529460291E-14,
-62.7787168150854));
#9798=CARTESIAN_POINT('Ctrl Pts',(-114.085205078271,1.09954677696283E-13,
-63.6554862616612));
#9799=CARTESIAN_POINT('Ctrl Pts',(-110.876720955829,3.88437234764698E-14,
-64.6815897913564));
#9800=CARTESIAN_POINT('Ctrl Pts',(-107.721164151354,6.31408343849688E-14,
-65.8535592808521));
#9801=CARTESIAN_POINT('Ctrl Pts',(-104.510754540394,7.27076390459741E-14,
-67.0459010277961));
#9802=CARTESIAN_POINT('Ctrl Pts',(-101.355129960864,2.13060038867633E-14,
-68.3892216824963));
#9803=CARTESIAN_POINT('Ctrl Pts',(-98.2651875381796,7.99960446463358E-14,
-69.8797997202865));
#9804=CARTESIAN_POINT('Ctrl Pts',(-95.141608011939,1.21775280556001E-13,
-71.3866041859377));
#9805=CARTESIAN_POINT('Ctrl Pts',(-92.0851458120254,4.16371041647899E-14,
-73.0438828741871));
#9806=CARTESIAN_POINT('Ctrl Pts',(-89.1070253835134,5.55641162014496E-14,
-74.847790689453));
#9807=CARTESIAN_POINT('Ctrl Pts',(-86.1168527340016,6.74633771530896E-14,
-76.6589987788935));
#9808=CARTESIAN_POINT('Ctrl Pts',(-83.2056472832252,1.97565378180188E-14,
-78.6180166790309));
#9809=CARTESIAN_POINT('Ctrl Pts',(-80.384830163582,3.31094929983044E-14,
-80.7210696683278));
#9810=CARTESIAN_POINT('Ctrl Pts',(-77.5611534148132,3.07519208876647E-14,
-82.8262546468059));
#9811=CARTESIAN_POINT('Ctrl Pts',(-74.8381140101429,6.55809408055033E-14,
-85.0685191399763));
#9812=CARTESIAN_POINT('Ctrl Pts',(-72.2297132774974,2.94546559451853E-14,
-87.4364962704631));
#9813=CARTESIAN_POINT('Ctrl Pts',(-69.6213194790229,1.09983012374116E-14,
-89.8044671059209));
#9814=CARTESIAN_POINT('Ctrl Pts',(-67.1275347240066,2.00661256494869E-14,
-92.2980716005061));
#9815=CARTESIAN_POINT('Ctrl Pts',(-64.7594023581046,4.44089209850063E-15,
-94.9062580231543));
#9816=CARTESIAN_POINT('Ctrl Pts',(-62.402101299093,1.71643312990407E-14,
-97.5025151854376));
#9817=CARTESIAN_POINT('Ctrl Pts',(-60.1698465605611,7.92727737594203E-14,
-100.211731774115));
#9818=CARTESIAN_POINT('Ctrl Pts',(-58.0726499521868,5.06167238114794E-14,
-103.021640804036));
#9819=CARTESIAN_POINT('Ctrl Pts',(-55.994832850032,1.08718014075603E-14,
-105.805584385938));
#9820=CARTESIAN_POINT('Ctrl Pts',(-54.0490749518659,-5.23372399894248E-14,
-108.689139472133));
#9821=CARTESIAN_POINT('Ctrl Pts',(-52.2449416359333,8.70188233993832E-15,
-111.658230646188));
#9822=CARTESIAN_POINT('Ctrl Pts',(-50.4652489916242,4.61267413567307E-14,
-114.587099414412));
#9823=CARTESIAN_POINT('Ctrl Pts',(-48.8232383526353,-3.96485956199284E-15,
-117.599305307977));
#9824=CARTESIAN_POINT('Ctrl Pts',(-47.3258881353928,-1.91641373722875E-14,
-120.682033527671));
#9825=CARTESIAN_POINT('Ctrl Pts',(-45.8550866032242,-8.76261135605058E-15,
-123.710103605448));
#9826=CARTESIAN_POINT('Ctrl Pts',(-44.5237168473911,9.44160675302571E-16,
-126.806759783349));
#9827=CARTESIAN_POINT('Ctrl Pts',(-43.3384647873199,3.63520113533591E-14,
-129.955904638828));
#9828=CARTESIAN_POINT('Ctrl Pts',(-42.178411369753,8.22686500091128E-14,
-133.03809818658));
#9829=CARTESIAN_POINT('Ctrl Pts',(-41.1578799651058,2.73842972706966E-14,
-136.171204882295));
#9830=CARTESIAN_POINT('Ctrl Pts',(-40.2800279987793,2.40516445328869E-14,
-139.345683225176));
#9831=CARTESIAN_POINT('Ctrl Pts',(-38.5944013814791,-4.43847532318893E-14,
-145.441227116471));
#9832=CARTESIAN_POINT('Ctrl Pts',(-37.4373840532588,1.49418878328148E-13,
-151.68681682945));
#9833=CARTESIAN_POINT('Ctrl Pts',(-36.827675631427,5.35189297393157E-14,
-157.982075177761));
#9834=CARTESIAN_POINT('',(-36.827675631427,-4.99999999999994,-157.982075177761));
#9835=CARTESIAN_POINT('Origin',(145.859521458148,-4.99999999999993,-168.542028553823));
#9836=CARTESIAN_POINT('',(36.8276756314269,6.20110919257889E-14,-157.98207517776));
#9837=CARTESIAN_POINT('Ctrl Pts',(145.859521458148,1.99966320462804E-14,
-59.));
#9838=CARTESIAN_POINT('Ctrl Pts',(145.635702363798,0.000231282957399252,
-59.));
#9839=CARTESIAN_POINT('Ctrl Pts',(145.411883255443,0.000447783508952677,
-59.0006859694082));
#9840=CARTESIAN_POINT('Ctrl Pts',(145.188067286725,0.000650024989461163,
-59.0020579084816));
#9841=CARTESIAN_POINT('Ctrl Pts',(139.052999252887,0.00619371005042004,
-59.0396644278098));
#9842=CARTESIAN_POINT('Ctrl Pts',(132.962545444417,-1.11887795632077E-13,
-59.592285658868));
#9843=CARTESIAN_POINT('Ctrl Pts',(126.977116946521,-1.04423077240787E-13,
-60.639707820922));
#9844=CARTESIAN_POINT('Ctrl Pts',(123.729336577944,-9.67014244773527E-14,
-61.2080542871319));
#9845=CARTESIAN_POINT('Ctrl Pts',(120.512481495576,-1.13587683266672E-13,
-61.9221153240646));
#9846=CARTESIAN_POINT('Ctrl Pts',(117.336234309904,-6.90972208920379E-14,
-62.7787168150856));
#9847=CARTESIAN_POINT('Ctrl Pts',(114.085205078283,-2.10873246295173E-14,
-63.6554862616581));
#9848=CARTESIAN_POINT('Ctrl Pts',(110.87672095584,-5.77851871173568E-14,
-64.6815897913523));
#9849=CARTESIAN_POINT('Ctrl Pts',(107.721164151354,-7.0435270368486E-14,
-65.8535592808523));
#9850=CARTESIAN_POINT('Ctrl Pts',(104.510754540406,-5.9941934650156E-14,
-67.0459010277919));
#9851=CARTESIAN_POINT('Ctrl Pts',(101.355129960875,-7.52622445179423E-14,
-68.389221682491));
#9852=CARTESIAN_POINT('Ctrl Pts',(98.2651875381795,-6.59048807687785E-14,
-69.8797997202867));
#9853=CARTESIAN_POINT('Ctrl Pts',(95.1416080119508,-2.09429382763629E-14,
-71.3866041859322));
#9854=CARTESIAN_POINT('Ctrl Pts',(92.0851458120368,-4.4049120057977E-14,
-73.0438828741804));
#9855=CARTESIAN_POINT('Ctrl Pts',(89.1070253835134,-1.83922193067957E-14,
-74.8477906894531));
#9856=CARTESIAN_POINT('Ctrl Pts',(86.1168527340136,-2.8634501446293E-14,
-76.6589987788863));
#9857=CARTESIAN_POINT('Ctrl Pts',(83.2056472832369,1.40408434793159E-14,
-78.6180166790223));
#9858=CARTESIAN_POINT('Ctrl Pts',(80.3848301635821,-1.04201332750223E-14,
-80.7210696683279));
#9859=CARTESIAN_POINT('Ctrl Pts',(77.561153414816,-2.03746625468862E-14,
-82.8262546468039));
#9860=CARTESIAN_POINT('Ctrl Pts',(74.8381140101453,-3.84257827749966E-14,
-85.0685191399742));
#9861=CARTESIAN_POINT('Ctrl Pts',(72.2297132774974,-4.91540503775017E-14,
-87.4364962704632));
#9862=CARTESIAN_POINT('Ctrl Pts',(69.6213194790202,-3.34285257340705E-14,
-89.8044671059234));
#9863=CARTESIAN_POINT('Ctrl Pts',(67.1275347240061,-1.45705862260143E-14,
-92.2980716005068));
#9864=CARTESIAN_POINT('Ctrl Pts',(64.7594023581046,-1.87525810038756E-14,
-94.9062580231544));
#9865=CARTESIAN_POINT('Ctrl Pts',(62.4021012990951,-1.76400073832052E-14,
-97.5025151854354));
#9866=CARTESIAN_POINT('Ctrl Pts',(60.1698465605618,-7.19881477211928E-14,
-100.211731774114));
#9867=CARTESIAN_POINT('Ctrl Pts',(58.0726499521868,-5.42214207492858E-14,
-103.021640804037));
#9868=CARTESIAN_POINT('Ctrl Pts',(55.994832850029,-2.90803087727514E-14,
-105.805584385943));
#9869=CARTESIAN_POINT('Ctrl Pts',(54.0490749518629,-7.79522172356907E-14,
-108.689139472138));
#9870=CARTESIAN_POINT('Ctrl Pts',(52.2449416359332,-1.01288911340345E-13,
-111.658230646188));
#9871=CARTESIAN_POINT('Ctrl Pts',(50.4652489916246,-1.2018699629012E-13,
-114.587099414412));
#9872=CARTESIAN_POINT('Ctrl Pts',(48.8232383526351,-2.65689998570122E-14,
-117.599305307977));
#9873=CARTESIAN_POINT('Ctrl Pts',(47.3258881353929,-8.66874694043732E-16,
-120.682033527671));
#9874=CARTESIAN_POINT('Ctrl Pts',(45.855086603224,4.04340402343437E-14,
-123.710103605448));
#9875=CARTESIAN_POINT('Ctrl Pts',(44.5237168473911,-2.2235983896746E-14,
-126.806759783349));
#9876=CARTESIAN_POINT('Ctrl Pts',(43.3384647873198,-8.23114176779849E-14,
-129.955904638828));
#9877=CARTESIAN_POINT('Ctrl Pts',(42.1784113697529,-1.68925830949098E-13,
-133.03809818658));
#9878=CARTESIAN_POINT('Ctrl Pts',(41.1578799651058,-8.85986346721827E-14,
-136.171204882295));
#9879=CARTESIAN_POINT('Ctrl Pts',(40.2800279987792,-4.7668540935266E-14,
-139.345683225176));
#9880=CARTESIAN_POINT('Ctrl Pts',(38.5944013814802,5.17415891553732E-14,
-145.441227116467));
#9881=CARTESIAN_POINT('Ctrl Pts',(37.4373840532589,8.01494831266999E-14,
-151.686816829449));
#9882=CARTESIAN_POINT('Ctrl Pts',(36.8276756314269,-5.35238086490919E-14,
-157.982075177761));
#9883=CARTESIAN_POINT('',(36.8276756314269,-4.99999999999994,-157.982075177761));
#9884=CARTESIAN_POINT('Origin',(-5.2737622621639E-14,-4.99999999999994,
-154.415240784856));
#9885=CARTESIAN_POINT('Ctrl Pts',(-36.827675631427,6.00431163122472E-14,
-157.982075177761));
#9886=CARTESIAN_POINT('Ctrl Pts',(-36.679749707944,6.07211040707748E-14,
-159.50941492147));
#9887=CARTESIAN_POINT('Ctrl Pts',(-36.4288634825458,6.14323406959253E-14,
-161.114741394618));
#9888=CARTESIAN_POINT('Ctrl Pts',(-36.0405708212051,6.21724893790088E-14,
-162.786456639301));
#9889=CARTESIAN_POINT('Ctrl Pts',(-35.6522781598644,6.07095392476017E-14,
-164.458171883983));
#9890=CARTESIAN_POINT('Ctrl Pts',(-35.1263043652441,6.14323406959253E-14,
-166.196602013066));
#9891=CARTESIAN_POINT('Ctrl Pts',(-34.4253505833174,6.21724893790088E-14,
-167.976038593823));
#9892=CARTESIAN_POINT('Ctrl Pts',(-33.7243968013906,6.95739762098431E-14,
-169.755475174581));
#9893=CARTESIAN_POINT('Ctrl Pts',(-32.8479279009937,7.03141248929266E-14,
-171.576162799206));
#9894=CARTESIAN_POINT('Ctrl Pts',(-31.7618111665596,7.105427357601E-14,
-173.393843247098));
#9895=CARTESIAN_POINT('Ctrl Pts',(-30.6756944321255,6.95508465634968E-14,
-175.21152369499));
#9896=CARTESIAN_POINT('Ctrl Pts',(-29.3791356772817,7.03141248929266E-14,
-177.026147945389));
#9897=CARTESIAN_POINT('Ctrl Pts',(-27.851210931603,7.105427357601E-14,-178.773197383129));
#9898=CARTESIAN_POINT('Ctrl Pts',(-26.3232861859243,6.96896244415749E-14,
-180.520246820869));
#9899=CARTESIAN_POINT('Ctrl Pts',(-24.563134662835,7.0406643478312E-14,
-182.199131371192));
#9900=CARTESIAN_POINT('Ctrl Pts',(-22.5757614892595,7.105427357601E-14,
-183.729656917197));
#9901=CARTESIAN_POINT('Ctrl Pts',(-20.588388315684,7.00250043135971E-14,
-185.260182463203));
#9902=CARTESIAN_POINT('Ctrl Pts',(-18.3733019437227,7.05916806490829E-14,
-186.64113254965));
#9903=CARTESIAN_POINT('Ctrl Pts',(-15.9720905535861,7.105427357601E-14,
-187.790266228263));
#9904=CARTESIAN_POINT('Ctrl Pts',(-13.5708791634495,7.92652980289669E-14,
-188.939399906875));
#9905=CARTESIAN_POINT('Ctrl Pts',(-10.9839174320017,7.9658502016855E-14,
-189.855200551742));
#9906=CARTESIAN_POINT('Ctrl Pts',(-8.29064013714815,7.99360577730113E-14,
-190.474432208352));
#9907=CARTESIAN_POINT('Ctrl Pts',(-5.59736284229463,7.97972798949331E-14,
-191.093663864962));
#9908=CARTESIAN_POINT('Ctrl Pts',(-2.79913386299203,7.99360577730113E-14,
-191.415240784856));
#9909=CARTESIAN_POINT('Ctrl Pts',(-5.19029264012261E-14,7.99360577730113E-14,
-191.415240784856));
#9910=CARTESIAN_POINT('Ctrl Pts',(2.79913386299191,8.03755210535921E-14,
-191.415240784856));
#9911=CARTESIAN_POINT('Ctrl Pts',(5.59736284229452,8.02136135291676E-14,
-191.093663864962));
#9912=CARTESIAN_POINT('Ctrl Pts',(8.29064013714802,7.99360577730113E-14,
-190.474432208352));
#9913=CARTESIAN_POINT('Ctrl Pts',(10.9839174320015,7.18753760213057E-14,
-189.855200551742));
#9914=CARTESIAN_POINT('Ctrl Pts',(13.5708791634494,7.15168665029372E-14,
-188.939399906875));
#9915=CARTESIAN_POINT('Ctrl Pts',(15.972090553586,7.105427357601E-14,-187.790266228263));
#9916=CARTESIAN_POINT('Ctrl Pts',(18.3733019437226,7.2280144832367E-14,
-186.64113254965));
#9917=CARTESIAN_POINT('Ctrl Pts',(20.5883883156839,7.1701903673708E-14,
-185.260182463203));
#9918=CARTESIAN_POINT('Ctrl Pts',(22.5757614892594,7.105427357601E-14,-183.729656917197));
#9919=CARTESIAN_POINT('Ctrl Pts',(24.5631346628349,7.25114412958305E-14,
-182.199131371191));
#9920=CARTESIAN_POINT('Ctrl Pts',(26.3232861859242,7.17944222590935E-14,
-180.520246820869));
#9921=CARTESIAN_POINT('Ctrl Pts',(27.8512109316029,7.105427357601E-14,-178.773197383129));
#9922=CARTESIAN_POINT('Ctrl Pts',(29.3791356772816,7.25345709421769E-14,
-177.026147945389));
#9923=CARTESIAN_POINT('Ctrl Pts',(30.6756944321254,7.17944222590935E-14,
-175.21152369499));
#9924=CARTESIAN_POINT('Ctrl Pts',(31.7618111665595,7.105427357601E-14,-173.393843247098));
#9925=CARTESIAN_POINT('Ctrl Pts',(32.8479279009936,6.36701339799354E-14,
-171.576162799206));
#9926=CARTESIAN_POINT('Ctrl Pts',(33.7243968013905,6.29126380620922E-14,
-169.755475174581));
#9927=CARTESIAN_POINT('Ctrl Pts',(34.4253505833173,6.21724893790088E-14,
-167.976038593823));
#9928=CARTESIAN_POINT('Ctrl Pts',(35.126304365244,6.36816988031086E-14,
-166.196602013066));
#9929=CARTESIAN_POINT('Ctrl Pts',(35.6522781598643,6.29126380620922E-14,
-164.458171883983));
#9930=CARTESIAN_POINT('Ctrl Pts',(36.040570821205,6.21724893790088E-14,
-162.786456639301));
#9931=CARTESIAN_POINT('Ctrl Pts',(36.4288634825457,6.36874812146952E-14,
-161.114741394618));
#9932=CARTESIAN_POINT('Ctrl Pts',(36.6797497079439,6.29126380620922E-14,
-159.509414921469));
#9933=CARTESIAN_POINT('Ctrl Pts',(36.8276756314269,6.21724893790088E-14,
-157.98207517776));
#9934=CARTESIAN_POINT('Ctrl Pts',(145.859521458148,1.99966320462804E-14,
-59.));
#9935=CARTESIAN_POINT('Ctrl Pts',(145.859521458148,1.99966320462804E-14,
-59.));
#9936=CARTESIAN_POINT('Ctrl Pts',(139.935495507955,1.08053483677362,-59.));
#9937=CARTESIAN_POINT('Ctrl Pts',(139.721849114916,-0.00946396581249335,
-59.));
#9938=CARTESIAN_POINT('Ctrl Pts',(134.282043748658,2.43566561952013,-59.));
#9939=CARTESIAN_POINT('Ctrl Pts',(133.377109516276,-0.0213330059978996,
-59.5229040505835));
#9940=CARTESIAN_POINT('Ctrl Pts',(126.153138109028,4.82540450931204,-59.));
#9941=CARTESIAN_POINT('Ctrl Pts',(123.752347114045,-0.0422637584217218,
-61.2196520084283));
#9942=CARTESIAN_POINT('Ctrl Pts',(123.502048229037,5.68149125852136,-59.));
#9943=CARTESIAN_POINT('Ctrl Pts',(120.52689037285,-0.0497618745872814,-61.9367613521045));
#9944=CARTESIAN_POINT('Ctrl Pts',(118.307860920989,7.50353712828284,-59.));
#9945=CARTESIAN_POINT('Ctrl Pts',(114.083064303984,-0.0657204343980337,
-63.6868647700364));
#9946=CARTESIAN_POINT('Ctrl Pts',(115.764763492932,8.469496248835,-59.));
#9947=CARTESIAN_POINT('Ctrl Pts',(110.864745391586,-0.0741808780432265,
-64.7198997778734));
#9948=CARTESIAN_POINT('Ctrl Pts',(110.777462874248,10.5021449940676,-59.));
#9949=CARTESIAN_POINT('Ctrl Pts',(104.480363411824,-0.0919840229109741,
-67.1072738686291));
#9950=CARTESIAN_POINT('Ctrl Pts',(108.33325968362,11.5688346187481,-59.));
#9951=CARTESIAN_POINT('Ctrl Pts',(101.314363689722,-0.101326724133529,-68.4616401636748));
#9952=CARTESIAN_POINT('Ctrl Pts',(103.53464932529,13.7938025050227,-59.));
#9953=CARTESIAN_POINT('Ctrl Pts',(95.0816761557438,-0.12081431425373,-71.488542771471));
#9954=CARTESIAN_POINT('Ctrl Pts',(101.180242157587,14.9520807666169,-59.));
#9955=CARTESIAN_POINT('Ctrl Pts',(92.01506006982,-0.130959203151376,-73.1610880645267));
#9956=CARTESIAN_POINT('Ctrl Pts',(96.5521256306011,17.3510840595046,-59.));
#9957=CARTESIAN_POINT('Ctrl Pts',(86.0280376851247,-0.151971098719488,-76.8121020395858));
#9958=CARTESIAN_POINT('Ctrl Pts',(94.2784162713182,18.591809090798,-59.));
#9959=CARTESIAN_POINT('Ctrl Pts',(83.1077052322228,-0.162838105389954,-78.7905587679407));
#9960=CARTESIAN_POINT('Ctrl Pts',(89.8025971466679,21.1465640558695,-59.));
#9961=CARTESIAN_POINT('Ctrl Pts',(77.4577804203387,-0.185214166601435,-83.032072624605));
#9962=CARTESIAN_POINT('Ctrl Pts',(87.6004873813004,22.4605939896476,-59.));
#9963=CARTESIAN_POINT('Ctrl Pts',(74.7282568958346,-0.19672322114245,-85.2950966600411));
#9964=CARTESIAN_POINT('Ctrl Pts',(83.2587692299763,25.152816892474,-59.));
#9965=CARTESIAN_POINT('Ctrl Pts',(69.499944269098,-0.220303308192758,-90.0760233255031));
#9966=CARTESIAN_POINT('Ctrl Pts',(81.1191608440196,26.5310098615222,-59.));
#9967=CARTESIAN_POINT('Ctrl Pts',(67.0012121106908,-0.232374340702051,-92.5938742603756));
#9968=CARTESIAN_POINT('Ctrl Pts',(76.8933472370124,29.3424169676743,-59.));
#9969=CARTESIAN_POINT('Ctrl Pts',(62.2680278295026,-0.256998313786643,-97.8476184497509));
#9970=CARTESIAN_POINT('Ctrl Pts',(74.8071420159619,30.7756311047781,-59.));
#9971=CARTESIAN_POINT('Ctrl Pts',(60.0336152811755,-0.269551254361943,-100.58344638055));
#9972=CARTESIAN_POINT('Ctrl Pts',(70.6790365242624,33.6879386798268,-59.));
#9973=CARTESIAN_POINT('Ctrl Pts',(55.8546997830352,-0.295058973676278,-106.230970575318));
#9974=CARTESIAN_POINT('Ctrl Pts',(68.6371362536135,35.1670321177717,-59.));
#9975=CARTESIAN_POINT('Ctrl Pts',(53.9102158500078,-0.308013752415314,-109.142594489691));
#9976=CARTESIAN_POINT('Ctrl Pts',(64.5885424482124,38.1619564272879,-59.));
#9977=CARTESIAN_POINT('Ctrl Pts',(50.3279822597621,-0.33424507815485,-115.096290916415));
#9978=CARTESIAN_POINT('Ctrl Pts',(62.5818489134604,39.6777872988593,-59.));
#9979=CARTESIAN_POINT('Ctrl Pts',(48.690230578512,-0.34752162515535,-118.13829117116));
#9980=CARTESIAN_POINT('Ctrl Pts',(58.5945703653485,42.7370446084141,-59.));
#9981=CARTESIAN_POINT('Ctrl Pts',(45.7292271162558,-0.374316417515544,-124.306271647363));
#9982=CARTESIAN_POINT('Ctrl Pts',(56.6139853519887,44.2804710463975,-58.9999999999999));
#9983=CARTESIAN_POINT('Ctrl Pts',(44.4059543564031,-0.387834662875238,-127.432186195309));
#9984=CARTESIAN_POINT('Ctrl Pts',(52.6698256321568,47.3857776215616,-58.9999999999999));
#9985=CARTESIAN_POINT('Ctrl Pts',(42.0729707249933,-0.415032782051548,-133.722570987114));
#9986=CARTESIAN_POINT('Ctrl Pts',(50.7062509256847,48.9476577587424,-58.9999999999999));
#9987=CARTESIAN_POINT('Ctrl Pts',(41.0632239705788,-0.428712655868165,-136.88698710447));
#9988=CARTESIAN_POINT('Ctrl Pts',(44.8273949448428,53.6472659182591,-58.9999999999999));
#9989=CARTESIAN_POINT('Ctrl Pts',(38.4911694101435,-0.469874615149992,-146.374221095626));
#9990=CARTESIAN_POINT('Ctrl Pts',(40.9239818090476,56.7989616885694,-58.9999999999999));
#9991=CARTESIAN_POINT('Ctrl Pts',(37.3884769401616,-0.49747903844718,-152.688287840106));
#9992=CARTESIAN_POINT('Ctrl Pts',(37.,59.9327136539873,-58.9999999999999));
#9993=CARTESIAN_POINT('Ctrl Pts',(36.8261663122663,-0.524926299244587,-158.849018976011));
#9994=CARTESIAN_POINT('Ctrl Pts',(37.,59.9327136539873,-58.9999999999999));
#9995=CARTESIAN_POINT('Ctrl Pts',(63.693153039627,38.6151528517792,-59.));
#9996=CARTESIAN_POINT('Ctrl Pts',(89.4344921389827,16.4672437121532,-59.));
#9997=CARTESIAN_POINT('Ctrl Pts',(125.680065601889,4.99999999980248,-59.));
#9998=CARTESIAN_POINT('',(37.,59.9327136539873,-58.9999999999999));
#9999=CARTESIAN_POINT('Ctrl Pts',(-37.,59.9327136539873,-58.9999999999999));
#10000=CARTESIAN_POINT('Ctrl Pts',(-36.826166311831,-0.524926450656172,
-158.849019226075));
#10001=CARTESIAN_POINT('Ctrl Pts',(-40.9239818090477,56.7989616885694,-58.9999999999999));
#10002=CARTESIAN_POINT('Ctrl Pts',(-37.3884769313072,-0.49747918194178,
-152.688288074741));
#10003=CARTESIAN_POINT('Ctrl Pts',(-44.8273949448429,53.6472659182591,-58.9999999999999));
#10004=CARTESIAN_POINT('Ctrl Pts',(-38.4911693942749,-0.469874750682276,
-146.374221314448));
#10005=CARTESIAN_POINT('Ctrl Pts',(-50.7062509256847,48.9476577587424,-58.9999999999999));
#10006=CARTESIAN_POINT('Ctrl Pts',(-41.0632239464286,-0.428712779527549,
-136.886987299532));
#10007=CARTESIAN_POINT('Ctrl Pts',(-52.6698256321568,47.3857776215616,-58.9999999999999));
#10008=CARTESIAN_POINT('Ctrl Pts',(-42.0729706984543,-0.415032901765061,
-133.722571174251));
#10009=CARTESIAN_POINT('Ctrl Pts',(-56.6139853519888,44.2804710463975,-58.9999999999999));
#10010=CARTESIAN_POINT('Ctrl Pts',(-44.405954325829,-0.38783477474363,-127.432186366692));
#10011=CARTESIAN_POINT('Ctrl Pts',(-58.5945703653485,42.7370446084141,-58.9999999999999));
#10012=CARTESIAN_POINT('Ctrl Pts',(-45.7292270840355,-0.374316525484686,
-124.306271810918));
#10013=CARTESIAN_POINT('Ctrl Pts',(-62.5818489134604,39.6777872988594,-58.9999999999999));
#10014=CARTESIAN_POINT('Ctrl Pts',(-48.6902305437215,-0.347521725395707,
-118.138291319267));
#10015=CARTESIAN_POINT('Ctrl Pts',(-64.5885424482125,38.1619564272879,-58.9999999999999));
#10016=CARTESIAN_POINT('Ctrl Pts',(-50.3279822240476,-0.334245174565673,
-115.096291056904));
#10017=CARTESIAN_POINT('Ctrl Pts',(-68.6371362536135,35.1670321177717,-58.9999999999999));
#10018=CARTESIAN_POINT('Ctrl Pts',(-53.9102158131253,-0.308013841259882,
-109.142594615269));
#10019=CARTESIAN_POINT('Ctrl Pts',(-70.6790365242624,33.6879386798268,-58.9999999999999));
#10020=CARTESIAN_POINT('Ctrl Pts',(-55.8546997459087,-0.295059058784125,
-106.230970693605));
#10021=CARTESIAN_POINT('Ctrl Pts',(-74.8071420159619,30.7756311047781,-58.9999999999999));
#10022=CARTESIAN_POINT('Ctrl Pts',(-60.0336152441763,-0.269551332112253,
-100.583446484693));
#10023=CARTESIAN_POINT('Ctrl Pts',(-76.8933472370124,29.3424169676743,-58.9999999999999));
#10024=CARTESIAN_POINT('Ctrl Pts',(-62.2680277928746,-0.256998387916139,
-97.8476185470417));
#10025=CARTESIAN_POINT('Ctrl Pts',(-81.1191608440196,26.5310098615222,-58.9999999999999));
#10026=CARTESIAN_POINT('Ctrl Pts',(-67.0012120753335,-0.232374407728921,
-92.5938743445089));
#10027=CARTESIAN_POINT('Ctrl Pts',(-83.2587692299763,25.152816892474,-58.9999999999999));
#10028=CARTESIAN_POINT('Ctrl Pts',(-69.49994423464,-0.220303371737818,-90.0760234033306));
#10029=CARTESIAN_POINT('Ctrl Pts',(-87.6004873813004,22.4605939896476,-58.9999999999999));
#10030=CARTESIAN_POINT('Ctrl Pts',(-74.7282568635971,-0.196723277885987,
-85.2950967258951));
#10031=CARTESIAN_POINT('Ctrl Pts',(-89.8025971466679,21.1465640558695,-58.9999999999999));
#10032=CARTESIAN_POINT('Ctrl Pts',(-77.4577803894221,-0.18521422002526,
-83.0320726847914));
#10033=CARTESIAN_POINT('Ctrl Pts',(-94.2784162713182,18.591809090798,-58.9999999999999));
#10034=CARTESIAN_POINT('Ctrl Pts',(-83.1077052042465,-0.162838152359549,
-78.7905588175045));
#10035=CARTESIAN_POINT('Ctrl Pts',(-96.5521256306011,17.3510840595046,-58.9999999999999));
#10036=CARTESIAN_POINT('Ctrl Pts',(-86.0280376587679,-0.151971142554565,
-76.8121020841948));
#10037=CARTESIAN_POINT('Ctrl Pts',(-101.180242157587,14.952080766617,-58.9999999999999));
#10038=CARTESIAN_POINT('Ctrl Pts',(-92.0150600468664,-0.130959240925708,
-73.161088099992));
#10039=CARTESIAN_POINT('Ctrl Pts',(-103.53464932529,13.7938025050227,-58.9999999999999));
#10040=CARTESIAN_POINT('Ctrl Pts',(-95.081676134574,-0.120814349101835,
-71.4885428027475));
#10041=CARTESIAN_POINT('Ctrl Pts',(-108.33325968362,11.5688346187481,-58.9999999999999));
#10042=CARTESIAN_POINT('Ctrl Pts',(-101.314363672144,-0.101326753360565,
-68.4616401873707));
#10043=CARTESIAN_POINT('Ctrl Pts',(-110.777462874248,10.5021449940676,-58.9999999999999));
#10044=CARTESIAN_POINT('Ctrl Pts',(-104.480363396053,-0.0919840494431687,
-67.1072738889331));
#10045=CARTESIAN_POINT('Ctrl Pts',(-115.764763492932,8.469496248835,-58.9999999999999));
#10046=CARTESIAN_POINT('Ctrl Pts',(-110.864745379315,-0.0741808994402193,
-64.7198997921983));
#10047=CARTESIAN_POINT('Ctrl Pts',(-118.307860920989,7.50353712828284,-58.9999999999999));
#10048=CARTESIAN_POINT('Ctrl Pts',(-114.083064293404,-0.0657204533546665,
-63.6868647817742));
#10049=CARTESIAN_POINT('Ctrl Pts',(-123.502048229037,5.68149125852135,-58.9999999999999));
#10050=CARTESIAN_POINT('Ctrl Pts',(-120.526890365399,-0.0497618889407711,
-61.9367613594593));
#10051=CARTESIAN_POINT('Ctrl Pts',(-126.153138109028,4.82540450931203,-58.9999999999999));
#10052=CARTESIAN_POINT('Ctrl Pts',(-123.752347108032,-0.0422637706124286,
-61.2196520139871));
#10053=CARTESIAN_POINT('Ctrl Pts',(-134.282043748658,2.43566561952013,-58.9999999999999));
#10054=CARTESIAN_POINT('Ctrl Pts',(-133.377109514009,-0.0213330121512667,
-59.522904051893));
#10055=CARTESIAN_POINT('Ctrl Pts',(-139.935495507955,1.08053483677361,-58.9999999999999));
#10056=CARTESIAN_POINT('Ctrl Pts',(-139.721849114381,-0.00946396854231285,
-58.9999999999999));
#10057=CARTESIAN_POINT('Ctrl Pts',(-145.859521458148,1.99966320462804E-14,
-58.9999999999999));
#10058=CARTESIAN_POINT('Ctrl Pts',(-145.859521458148,1.99966320462804E-14,
-58.9999999999999));
#10059=CARTESIAN_POINT('Ctrl Pts',(-125.680065601889,4.99999999980248,-58.9999999999999));
#10060=CARTESIAN_POINT('Ctrl Pts',(-89.4344921389829,16.4672437121532,-58.9999999999999));
#10061=CARTESIAN_POINT('Ctrl Pts',(-63.693153039627,38.6151528517792,-58.9999999999999));
#10062=CARTESIAN_POINT('Ctrl Pts',(-37.,59.9327136539873,-58.9999999999999));
#10063=CARTESIAN_POINT('',(-36.827675631427,6.00431163122472E-14,-157.982075177761));
#10064=CARTESIAN_POINT('Ctrl Pts',(37.,59.9327136539873,-58.9999999999999));
#10065=CARTESIAN_POINT('Ctrl Pts',(36.8276756314269,6.20110919257889E-14,
-157.98207517776));
#10066=CARTESIAN_POINT('Ctrl Pts',(35.962058784555,61.0726321354551,-58.9999999999999));
#10067=CARTESIAN_POINT('Ctrl Pts',(36.6797497079439,6.26598839444921E-14,
-159.50941492147));
#10068=CARTESIAN_POINT('Ctrl Pts',(34.8494287906845,62.1881303927957,-58.9999999999999));
#10069=CARTESIAN_POINT('Ctrl Pts',(36.4288634825457,6.33418036074103E-14,
-161.114741394618));
#10070=CARTESIAN_POINT('Ctrl Pts',(32.4772932645476,64.3449801372208,-58.9999999999999));
#10071=CARTESIAN_POINT('Ctrl Pts',(35.6522781598643,6.47620449293057E-14,
-164.458171883983));
#10072=CARTESIAN_POINT('Ctrl Pts',(31.2177877322813,65.3863316243053,-58.9999999999999));
#10073=CARTESIAN_POINT('Ctrl Pts',(35.126304365244,6.55005051163517E-14,
-166.196602013066));
#10074=CARTESIAN_POINT('Ctrl Pts',(28.5544031478084,67.3695815062162,-58.9999999999999));
#10075=CARTESIAN_POINT('Ctrl Pts',(33.7243968013905,6.70122633955936E-14,
-169.755475174581));
#10076=CARTESIAN_POINT('Ctrl Pts',(27.1503938737515,68.3111074622806,-58.9999999999999));
#10077=CARTESIAN_POINT('Ctrl Pts',(32.8479279009936,6.77856653870456E-14,
-171.576162799206));
#10078=CARTESIAN_POINT('Ctrl Pts',(24.2115292157522,70.0684707648055,-58.9999999999999));
#10079=CARTESIAN_POINT('Ctrl Pts',(30.6756944321254,6.93299145588525E-14,
-175.21152369499));
#10080=CARTESIAN_POINT('Ctrl Pts',(22.6766738318099,70.8843081112658,-58.9999999999999));
#10081=CARTESIAN_POINT('Ctrl Pts',(29.3791356772816,7.01007409158914E-14,
-177.026147945389));
#10082=CARTESIAN_POINT('Ctrl Pts',(19.4899048077957,72.3648035547606,-58.9999999999999));
#10083=CARTESIAN_POINT('Ctrl Pts',(26.3232861859242,7.15849840073899E-14,
-180.520246820869));
#10084=CARTESIAN_POINT('Ctrl Pts',(17.8381180298111,73.0290133496626,-58.9999999999999));
#10085=CARTESIAN_POINT('Ctrl Pts',(24.5631346628349,7.22981500865543E-14,
-182.199131371191));
#10086=CARTESIAN_POINT('Ctrl Pts',(14.4429405853757,74.1860012886773,-58.9999999999999));
#10087=CARTESIAN_POINT('Ctrl Pts',(20.5883883156839,7.35984406902132E-14,
-185.260182463203));
#10088=CARTESIAN_POINT('Ctrl Pts',(12.6995499189248,74.6787794327899,-58.9999999999999));
#10089=CARTESIAN_POINT('Ctrl Pts',(18.3733019437226,7.41850484819666E-14,
-186.64113254965));
#10090=CARTESIAN_POINT('Ctrl Pts',(9.14636534104551,75.473548273127,-58.9999999999999));
#10091=CARTESIAN_POINT('Ctrl Pts',(13.5708791634494,7.51613194945917E-14,
-188.939399906875));
#10092=CARTESIAN_POINT('Ctrl Pts',(7.33698151150069,75.775223998754,-58.9999999999999));
#10093=CARTESIAN_POINT('Ctrl Pts',(10.9839174320015,7.55503384745273E-14,
-189.855200551742));
#10094=CARTESIAN_POINT('Ctrl Pts',(3.6851544189294,76.1798832399239,-58.9999999999999));
#10095=CARTESIAN_POINT('Ctrl Pts',(5.59736284229452,7.60764199284953E-14,
-191.093663864962));
#10096=CARTESIAN_POINT('Ctrl Pts',(1.84271115590294,76.2828667554667,-58.9999999999999));
#10097=CARTESIAN_POINT('Ctrl Pts',(2.79913386299191,7.62130211921539E-14,
-191.415240784856));
#10098=CARTESIAN_POINT('Ctrl Pts',(-1.84271115590296,76.2828667554667,-58.9999999999999));
#10099=CARTESIAN_POINT('Ctrl Pts',(-2.79913386299203,7.62130211921539E-14,
-191.415240784856));
#10100=CARTESIAN_POINT('Ctrl Pts',(-3.68515441892943,76.1798832399239,-58.9999999999999));
#10101=CARTESIAN_POINT('Ctrl Pts',(-5.59736284229463,7.60764199284953E-14,
-191.093663864962));
#10102=CARTESIAN_POINT('Ctrl Pts',(-7.33698151150072,75.775223998754,-58.9999999999999));
#10103=CARTESIAN_POINT('Ctrl Pts',(-10.9839174320017,7.55503384745273E-14,
-189.855200551742));
#10104=CARTESIAN_POINT('Ctrl Pts',(-9.14636534104554,75.473548273127,-58.9999999999999));
#10105=CARTESIAN_POINT('Ctrl Pts',(-13.5708791634495,7.51613194945917E-14,
-188.939399906875));
#10106=CARTESIAN_POINT('Ctrl Pts',(-12.6995499189249,74.6787794327899,-58.9999999999999));
#10107=CARTESIAN_POINT('Ctrl Pts',(-18.3733019437227,7.41850484819666E-14,
-186.64113254965));
#10108=CARTESIAN_POINT('Ctrl Pts',(-14.4429405853757,74.1860012886773,-58.9999999999999));
#10109=CARTESIAN_POINT('Ctrl Pts',(-20.588388315684,7.35984406902132E-14,
-185.260182463203));
#10110=CARTESIAN_POINT('Ctrl Pts',(-17.8381180298111,73.0290133496626,-58.9999999999999));
#10111=CARTESIAN_POINT('Ctrl Pts',(-24.563134662835,7.22981500865543E-14,
-182.199131371192));
#10112=CARTESIAN_POINT('Ctrl Pts',(-19.4899048077957,72.3648035547606,-58.9999999999999));
#10113=CARTESIAN_POINT('Ctrl Pts',(-26.3232861859243,7.15849840073899E-14,
-180.520246820869));
#10114=CARTESIAN_POINT('Ctrl Pts',(-22.6766738318099,70.8843081112659,-58.9999999999999));
#10115=CARTESIAN_POINT('Ctrl Pts',(-29.3791356772817,7.01007409158914E-14,
-177.026147945389));
#10116=CARTESIAN_POINT('Ctrl Pts',(-24.2115292157522,70.0684707648055,-58.9999999999999));
#10117=CARTESIAN_POINT('Ctrl Pts',(-30.6756944321255,6.93299145588525E-14,
-175.21152369499));
#10118=CARTESIAN_POINT('Ctrl Pts',(-27.1503938737515,68.3111074622807,-58.9999999999999));
#10119=CARTESIAN_POINT('Ctrl Pts',(-32.8479279009937,6.77856653870456E-14,
-171.576162799206));
#10120=CARTESIAN_POINT('Ctrl Pts',(-28.5544031478085,67.3695815062162,-58.9999999999999));
#10121=CARTESIAN_POINT('Ctrl Pts',(-33.7243968013906,6.70122633955936E-14,
-169.755475174581));
#10122=CARTESIAN_POINT('Ctrl Pts',(-31.2177877322813,65.3863316243053,-58.9999999999999));
#10123=CARTESIAN_POINT('Ctrl Pts',(-35.1263043652441,6.55005051163517E-14,
-166.196602013066));
#10124=CARTESIAN_POINT('Ctrl Pts',(-32.4772932645476,64.3449801372209,-58.9999999999999));
#10125=CARTESIAN_POINT('Ctrl Pts',(-35.6522781598644,6.47620449293057E-14,
-164.458171883983));
#10126=CARTESIAN_POINT('Ctrl Pts',(-34.8494287906845,62.1881303927957,-58.9999999999999));
#10127=CARTESIAN_POINT('Ctrl Pts',(-36.4288634825458,6.33418036074103E-14,
-161.114741394618));
#10128=CARTESIAN_POINT('Ctrl Pts',(-35.9620587845551,61.0726321354551,-58.9999999999999));
#10129=CARTESIAN_POINT('Ctrl Pts',(-36.679749707944,6.26598839444921E-14,
-159.50941492147));
#10130=CARTESIAN_POINT('Ctrl Pts',(-37.,59.9327136539873,-58.9999999999999));
#10131=CARTESIAN_POINT('Ctrl Pts',(-36.827675631427,6.20110919257889E-14,
-157.982075177761));
#10132=CARTESIAN_POINT('Ctrl Pts',(-126.333741428594,4.79470864732773,-48.9999999999999));
#10133=CARTESIAN_POINT('Ctrl Pts',(-126.333741428594,4.79470864732774,-61.));
#10134=CARTESIAN_POINT('Ctrl Pts',(-89.743409874819,16.2013907644503,-48.9999999999999));
#10135=CARTESIAN_POINT('Ctrl Pts',(-89.743409874819,16.2013907644503,-61.));
#10136=CARTESIAN_POINT('Ctrl Pts',(-63.8533409643457,38.4872243219462,-48.9999999999999));
#10137=CARTESIAN_POINT('Ctrl Pts',(-63.8533409643457,38.4872243219462,-61.));
#10138=CARTESIAN_POINT('Ctrl Pts',(-37.,59.9327136539873,-48.9999999999999));
#10139=CARTESIAN_POINT('Ctrl Pts',(-37.,59.9327136539873,-61.));
#10140=CARTESIAN_POINT('Ctrl Pts',(37.,59.9327136539873,-48.9999999999999));
#10141=CARTESIAN_POINT('Ctrl Pts',(37.,59.9327136539873,-60.9999999999999));
#10142=CARTESIAN_POINT('Ctrl Pts',(63.8533446472751,38.4872213807023,-49.));
#10143=CARTESIAN_POINT('Ctrl Pts',(63.8533446472751,38.4872213807023,-61.));
#10144=CARTESIAN_POINT('Ctrl Pts',(89.7434169764527,16.2013846514567,-49.));
#10145=CARTESIAN_POINT('Ctrl Pts',(89.7434169764527,16.2013846514567,-61.));
#10146=CARTESIAN_POINT('Ctrl Pts',(126.333756483661,4.79470395405706,-49.));
#10147=CARTESIAN_POINT('Ctrl Pts',(126.333756483661,4.79470395405707,-61.));
#10148=CARTESIAN_POINT('Origin',(-20.,72.1122755947453,-130.738895837426));
#10149=CARTESIAN_POINT('',(-20.,54.6122755947453,5.50000000000008));
#10150=CARTESIAN_POINT('Origin',(-20.,54.6122755947453,-11.9999999999999));
#10151=CARTESIAN_POINT('Origin',(-20.,54.6122755947453,-11.9999999999999));
#10152=CARTESIAN_POINT('Origin',(20.,5.00000000109418,-130.738895837426));
#10153=CARTESIAN_POINT('',(20.,54.6122755947453,-29.4999999999999));
#10154=CARTESIAN_POINT('Origin',(20.,54.6122755947453,-11.9999999999999));
#10155=CARTESIAN_POINT('Origin',(20.,54.6122755947453,-11.9999999999999));
#10156=CARTESIAN_POINT('Origin',(-45.,54.6122755947453,-11.9999999999999));
#10157=CARTESIAN_POINT('',(-45.,54.6122755947453,5.50000000000008));
#10158=CARTESIAN_POINT('',(-45.,54.6122755947453,5.50000000000008));
#10159=CARTESIAN_POINT('Origin',(-45.,54.6122755947453,-11.9999999999999));
#10160=CARTESIAN_POINT('Origin',(-45.,54.6122755947453,-11.9999999999999));
#10161=CARTESIAN_POINT('',(-45.,54.6122755947453,-25.8975067682909));
#10162=CARTESIAN_POINT('Origin',(-45.,54.6122755947453,-11.9999999999999));
#10163=CARTESIAN_POINT('Origin',(45.,54.6122755947453,-11.9999999999999));
#10164=CARTESIAN_POINT('',(45.,54.6122755947453,-29.4999999999999));
#10165=CARTESIAN_POINT('',(45.,54.6122755947453,-29.4999999999999));
#10166=CARTESIAN_POINT('Origin',(45.,54.6122755947453,-11.9999999999999));
#10167=CARTESIAN_POINT('Origin',(45.,54.6122755947453,-11.9999999999999));
#10168=CARTESIAN_POINT('Origin',(165.591979774207,54.6122755947453,-12.));
#10169=CARTESIAN_POINT('',(165.591979774207,54.6122755947453,-25.8975067682909));
#10170=CARTESIAN_POINT('Origin',(0.,89.,-11.9999999999999));
#10171=CARTESIAN_POINT('',(-2.44929359829471E-15,89.,-31.9999999999999));
#10172=CARTESIAN_POINT('Origin',(0.,89.,-11.9999999999999));
#10173=CARTESIAN_POINT('Origin',(0.,-5.00102500000001,-11.9999999999999));
#10174=CARTESIAN_POINT('',(-2.44929359829471E-15,-5.00102500000001,-31.9999999999999));
#10175=CARTESIAN_POINT('Origin',(0.,29.,-11.9999999999999));
#10176=CARTESIAN_POINT('Origin',(65.6680057154831,-5.,25.0000000000001));
#10177=CARTESIAN_POINT('Origin',(-65.6680057154831,-5.,25.0000000000001));
#10178=CARTESIAN_POINT('Origin',(-142.322386603279,-5.000025,-11.9999999999999));
#10179=CARTESIAN_POINT('',(-142.322386603279,-5.000025,-15.9999999999999));
#10180=CARTESIAN_POINT('Origin',(-115.629992744845,-5.000025,-11.9999999999999));
#10181=CARTESIAN_POINT('',(-115.629992744845,-5.000025,-27.9631510575948));
#10182=CARTESIAN_POINT('Origin',(-88.9375988864104,-5.000025,-11.9999999999999));
#10183=CARTESIAN_POINT('',(-88.9375988864104,-5.000025,-15.9999999999999));
#10184=CARTESIAN_POINT('Origin',(142.322386603279,-5.000025,-11.9999999999999));
#10185=CARTESIAN_POINT('',(142.322386603279,-5.000025,-15.9999999999999));
#10186=CARTESIAN_POINT('Origin',(115.629992744845,-5.000025,-11.9999999999999));
#10187=CARTESIAN_POINT('',(115.629992744845,-5.000025,-27.9631510575948));
#10188=CARTESIAN_POINT('Origin',(88.9375988864104,-5.000025,-11.9999999999999));
#10189=CARTESIAN_POINT('',(88.9375988864104,-5.000025,-15.9999999999999));
#10190=CARTESIAN_POINT('',(0.,0.,0.));
#10191=CARTESIAN_POINT('Origin',(50.,54.6122755947453,-11.9999999999999));
#10192=CARTESIAN_POINT('',(36.,54.6122755947453,-32.4999999999999));
#10193=CARTESIAN_POINT('',(36.,54.6122755947453,8.50000000000008));
#10194=CARTESIAN_POINT('Origin',(36.,54.6122755947453,-11.9999999999999));
#10195=CARTESIAN_POINT('Origin',(36.,54.6122755947453,-11.9999999999999));
#10196=CARTESIAN_POINT('',(36.603289189263,54.6122755947453,-32.4999999999999));
#10197=CARTESIAN_POINT('',(50.,54.6122755947453,-32.4999999999999));
#10198=CARTESIAN_POINT('',(36.7497490222913,54.2658144588871,-32.4970721002132));
#10199=CARTESIAN_POINT('Ctrl Pts',(36.7497490222914,54.2658144588871,-32.4970721002132));
#10200=CARTESIAN_POINT('Ctrl Pts',(36.7079677621958,54.3157388332819,-32.4979159697851));
#10201=CARTESIAN_POINT('Ctrl Pts',(36.6713203406449,54.3700115492414,-32.4986487617911));
#10202=CARTESIAN_POINT('Ctrl Pts',(36.6219970312668,54.4788517884076,-32.4996303938589));
#10203=CARTESIAN_POINT('Ctrl Pts',(36.6075439138862,54.5320464525539,-32.4999158675413));
#10204=CARTESIAN_POINT('Ctrl Pts',(36.6035546196614,54.5952824394035,-32.4999947523746));
#10205=CARTESIAN_POINT('Ctrl Pts',(36.6032891892631,54.6038064661215,-32.4999999999999));
#10206=CARTESIAN_POINT('Ctrl Pts',(36.6032891892631,54.6122755947453,-32.4999999999999));
#10207=CARTESIAN_POINT('',(48.396710810737,54.6122755947453,-32.4999999999999));
#10208=CARTESIAN_POINT('Ctrl Pts',(48.396710810737,54.6122755947453,-32.4999999999999));
#10209=CARTESIAN_POINT('Ctrl Pts',(48.396710810737,54.5998907719614,-32.4999999999999));
#10210=CARTESIAN_POINT('Ctrl Pts',(48.3961431217452,54.5874935361619,-32.4999887774468));
#10211=CARTESIAN_POINT('Ctrl Pts',(48.3891968128691,54.5117737928711,-32.4998514003519));
#10212=CARTESIAN_POINT('Ctrl Pts',(48.3690498018801,54.4529115279532,-32.4994531179785));
#10213=CARTESIAN_POINT('Ctrl Pts',(48.2945766533058,54.3105701888654,-32.49796779174));
#10214=CARTESIAN_POINT('Ctrl Pts',(48.224634010684,54.229506699135,-32.4965615873769));
#10215=CARTESIAN_POINT('Ctrl Pts',(47.9894682579553,54.0138621012104,-32.4917505532513));
#10216=CARTESIAN_POINT('Ctrl Pts',(47.790194476128,53.8921934273276,-32.4875698440548));
#10217=CARTESIAN_POINT('Ctrl Pts',(47.2591893370102,53.6095844257818,-32.4763245946928));
#10218=CARTESIAN_POINT('Ctrl Pts',(46.8036941106391,53.4296399345416,-32.4664417842137));
#10219=CARTESIAN_POINT('Ctrl Pts',(44.8908589619487,52.8583430003526,-32.4291083452159));
#10220=CARTESIAN_POINT('Ctrl Pts',(43.0234357271856,52.6236088262441,-32.4042961436254));
#10221=CARTESIAN_POINT('Ctrl Pts',(39.8390803845175,52.9459866017737,-32.4325402594283));
#10222=CARTESIAN_POINT('Ctrl Pts',(38.8321900018614,53.205505452804,-32.4535208321079));
#10223=CARTESIAN_POINT('Ctrl Pts',(37.7302514044692,53.6201478825653,-32.476460031332));
#10224=CARTESIAN_POINT('Ctrl Pts',(37.4193174431745,53.768280734008,-32.483158770581));
#10225=CARTESIAN_POINT('Ctrl Pts',(37.0379364071817,54.0043124559943,-32.4911694687953));
#10226=CARTESIAN_POINT('Ctrl Pts',(36.8894774405333,54.1120017210872,-32.4942401368472));
#10227=CARTESIAN_POINT('Ctrl Pts',(36.7699059821373,54.2423162108141,-32.4966645914004));
#10228=CARTESIAN_POINT('Ctrl Pts',(36.7596837012345,54.25394352369,-32.4968714463016));
#10229=CARTESIAN_POINT('Ctrl Pts',(36.7497490222914,54.2658144588871,-32.4970721002132));
#10230=CARTESIAN_POINT('',(49.,54.6122755947453,-32.4999999999999));
#10231=CARTESIAN_POINT('',(50.,54.6122755947453,-32.4999999999999));
#10232=CARTESIAN_POINT('',(49.,54.6122755947453,8.50000000000009));
#10233=CARTESIAN_POINT('Origin',(49.,54.6122755947453,-11.9999999999999));
#10234=CARTESIAN_POINT('Origin',(49.,54.6122755947453,-11.9999999999999));
#10235=CARTESIAN_POINT('Ctrl Pts',(36.603289189263,54.6122755947453,-32.4999999999999));
#10236=CARTESIAN_POINT('Ctrl Pts',(36.603289189263,54.6608249084485,-32.4999999999999));
#10237=CARTESIAN_POINT('Ctrl Pts',(36.6119924398781,54.7075701848921,-32.4998281802077));
#10238=CARTESIAN_POINT('Ctrl Pts',(36.6545156775753,54.8307810795885,-32.4989841905835));
#10239=CARTESIAN_POINT('Ctrl Pts',(36.7008380045797,54.9008048487387,-32.4980603157128));
#10240=CARTESIAN_POINT('Ctrl Pts',(36.8625317111402,55.0923640981108,-32.4947934283504));
#10241=CARTESIAN_POINT('Ctrl Pts',(37.0198338309866,55.2093236387767,-32.4915503477017));
#10242=CARTESIAN_POINT('Ctrl Pts',(37.4320685633155,55.4637121723344,-32.482889935361));
#10243=CARTESIAN_POINT('Ctrl Pts',(37.7488381293379,55.611880231403,-32.4760684685696));
#10244=CARTESIAN_POINT('Ctrl Pts',(39.1601676320809,56.1410407225304,-32.4467069002989));
#10245=CARTESIAN_POINT('Ctrl Pts',(40.717083195287,56.4741768433207,-32.4152718262714));
#10246=CARTESIAN_POINT('Ctrl Pts',(42.5,56.4741768433207,-32.4152718262714));
#10247=CARTESIAN_POINT('Ctrl Pts',(43.4574590376155,56.4741768433207,-32.4152718262714));
#10248=CARTESIAN_POINT('Ctrl Pts',(44.4269153217986,56.3794041517536,-32.4246324531227));
#10249=CARTESIAN_POINT('Ctrl Pts',(46.1871857836264,56.0096519365651,-32.4530673729712));
#10250=CARTESIAN_POINT('Ctrl Pts',(46.8757138664064,55.7779082090869,-32.4681777143441));
#10251=CARTESIAN_POINT('Ctrl Pts',(47.6009912659702,55.4395958991355,-32.4835638316369));
#10252=CARTESIAN_POINT('Ctrl Pts',(47.8399918525533,55.309998820274,-32.4886343233478));
#10253=CARTESIAN_POINT('Ctrl Pts',(48.1243771925797,55.091934993814,-32.4945190874943));
#10254=CARTESIAN_POINT('Ctrl Pts',(48.2195690308988,55.0050263124739,-32.4964575266732));
#10255=CARTESIAN_POINT('Ctrl Pts',(48.3274797628088,54.8557541081654,-32.4986259493983));
#10256=CARTESIAN_POINT('Ctrl Pts',(48.3595242538026,54.796889883988,-32.4992631372541));
#10257=CARTESIAN_POINT('Ctrl Pts',(48.3905089403897,54.6939813738137,-32.4998775530034));
#10258=CARTESIAN_POINT('Ctrl Pts',(48.396710810737,54.6531962409273,-32.4999999999999));
#10259=CARTESIAN_POINT('Ctrl Pts',(48.396710810737,54.6122755947453,-32.4999999999999));
#10260=CARTESIAN_POINT('',(36.5,41.5141044679107,3.76984188672031));
#10261=CARTESIAN_POINT('',(48.5,41.5141044679107,3.76984188672031));
#10262=CARTESIAN_POINT('',(48.5,41.5141044679107,3.76984188672031));
#10263=CARTESIAN_POINT('',(48.5,38.8424337080254,1.09817112683513));
#10264=CARTESIAN_POINT('Origin',(48.5,54.6122755947453,-11.9999999999999));
#10265=CARTESIAN_POINT('',(36.5,38.8424337080254,1.09817112683513));
#10266=CARTESIAN_POINT('',(48.5,38.8424337080254,1.09817112683513));
#10267=CARTESIAN_POINT('Origin',(36.5,54.6122755947453,-11.9999999999999));
#10268=CARTESIAN_POINT('',(36.5,38.8424337080252,-25.0981711268347));
#10269=CARTESIAN_POINT('',(48.5,38.8424337080252,-25.0981711268347));
#10270=CARTESIAN_POINT('',(48.5,38.8424337080252,-25.0981711268347));
#10271=CARTESIAN_POINT('',(48.5,41.5141044679105,-27.7698418867199));
#10272=CARTESIAN_POINT('Origin',(48.5,54.6122755947453,-11.9999999999999));
#10273=CARTESIAN_POINT('',(36.5,41.5141044679105,-27.7698418867199));
#10274=CARTESIAN_POINT('',(48.5,41.5141044679105,-27.7698418867199));
#10275=CARTESIAN_POINT('Origin',(36.5,54.6122755947453,-11.9999999999999));
#10276=CARTESIAN_POINT('',(36.5,67.7104467215801,-27.7698418867201));
#10277=CARTESIAN_POINT('',(48.5,67.7104467215801,-27.7698418867201));
#10278=CARTESIAN_POINT('',(48.5,67.7104467215801,-27.7698418867201));
#10279=CARTESIAN_POINT('',(48.5,70.3821174814653,-25.0981711268349));
#10280=CARTESIAN_POINT('Origin',(48.5,54.6122755947453,-11.9999999999999));
#10281=CARTESIAN_POINT('',(36.5,70.3821174814653,-25.0981711268349));
#10282=CARTESIAN_POINT('',(48.5,70.3821174814653,-25.0981711268349));
#10283=CARTESIAN_POINT('Origin',(36.5,54.6122755947453,-11.9999999999999));
#10284=CARTESIAN_POINT('',(36.5,70.3821174814654,1.09817112683487));
#10285=CARTESIAN_POINT('',(48.5,70.3821174814654,1.09817112683488));
#10286=CARTESIAN_POINT('',(48.5,70.3821174814654,1.09817112683488));
#10287=CARTESIAN_POINT('',(48.5,67.7104467215802,3.76984188672011));
#10288=CARTESIAN_POINT('Origin',(48.5,54.6122755947453,-11.9999999999999));
#10289=CARTESIAN_POINT('',(36.5,67.7104467215802,3.76984188672011));
#10290=CARTESIAN_POINT('',(48.5,67.7104467215802,3.76984188672011));
#10291=CARTESIAN_POINT('Origin',(36.5,54.6122755947453,-11.9999999999999));
#10292=CARTESIAN_POINT('',(36.7497652551312,75.1093469933142,-12.3464475251848));
#10293=CARTESIAN_POINT('Ctrl Pts',(42.5,75.0275474210168,-13.8619012485751));
#10294=CARTESIAN_POINT('Ctrl Pts',(41.5425409623847,75.0275474210168,-13.8619012485751));
#10295=CARTESIAN_POINT('Ctrl Pts',(40.5730846782014,75.0369080478681,-13.767128557008));
#10296=CARTESIAN_POINT('Ctrl Pts',(38.8128142163727,75.0653429677166,-13.3973763418193));
#10297=CARTESIAN_POINT('Ctrl Pts',(38.124286133593,75.0804533090896,-13.165632614341));
#10298=CARTESIAN_POINT('Ctrl Pts',(37.39900873403,75.0958394263824,-12.82732030439));
#10299=CARTESIAN_POINT('Ctrl Pts',(37.1600081474468,75.1009099180932,-12.6977232255284));
#10300=CARTESIAN_POINT('Ctrl Pts',(36.8756228074202,75.1067946822398,-12.4796593990683));
#10301=CARTESIAN_POINT('Ctrl Pts',(36.7804309691012,75.1087331214186,-12.3927507177283));
#10302=CARTESIAN_POINT('Ctrl Pts',(36.6725202371911,75.1109015441437,-12.2434785134197));
#10303=CARTESIAN_POINT('Ctrl Pts',(36.6404757461974,75.1115387319995,-12.1846142892423));
#10304=CARTESIAN_POINT('Ctrl Pts',(36.60578337376,75.1122266698925,-12.0693915532655));
#10305=CARTESIAN_POINT('Ctrl Pts',(36.6000950949635,75.1123387689502,-12.0162240743446));
#10306=CARTESIAN_POINT('Ctrl Pts',(36.6108031871309,75.1121269950974,-11.8994981981255));
#10307=CARTESIAN_POINT('Ctrl Pts',(36.63095019812,75.1117287127239,-11.8406359332075));
#10308=CARTESIAN_POINT('Ctrl Pts',(36.705423346694,75.1102433864854,-11.6982945941202));
#10309=CARTESIAN_POINT('Ctrl Pts',(36.7753659893155,75.1088371821223,-11.6172311043898));
#10310=CARTESIAN_POINT('Ctrl Pts',(37.0105317420447,75.1040261479967,-11.4015865064648));
#10311=CARTESIAN_POINT('Ctrl Pts',(37.2098055238719,75.0998454388001,-11.279917832582));
#10312=CARTESIAN_POINT('Ctrl Pts',(37.7408106629901,75.0886001894382,-10.997308831036));
#10313=CARTESIAN_POINT('Ctrl Pts',(38.1963058893614,75.0787173789591,-10.8173643397959));
#10314=CARTESIAN_POINT('Ctrl Pts',(40.1091410380511,75.0413839399612,-10.2460674056071));
#10315=CARTESIAN_POINT('Ctrl Pts',(41.9765642728142,75.0165717383708,-10.0113332314985));
#10316=CARTESIAN_POINT('Ctrl Pts',(45.1609196154824,75.0448158541737,-10.3337110070281));
#10317=CARTESIAN_POINT('Ctrl Pts',(46.1678099981386,75.0657964268533,-10.5932298580583));
#10318=CARTESIAN_POINT('Ctrl Pts',(47.2697485955313,75.0887356260774,-11.0078722878199));
#10319=CARTESIAN_POINT('Ctrl Pts',(47.5806825568259,75.0954343653265,-11.1560051392625));
#10320=CARTESIAN_POINT('Ctrl Pts',(47.9620635928186,75.1034450635407,-11.3920368612488));
#10321=CARTESIAN_POINT('Ctrl Pts',(48.1105225594667,75.1065157315926,-11.4997261263416));
#10322=CARTESIAN_POINT('Ctrl Pts',(48.2739688645561,75.10982980122,-11.6778574474043));
#10323=CARTESIAN_POINT('Ctrl Pts',(48.3224965288387,75.1108012999275,-11.7440918293815));
#10324=CARTESIAN_POINT('Ctrl Pts',(48.3780029687331,75.1119059886043,-11.8665761936618));
#10325=CARTESIAN_POINT('Ctrl Pts',(48.3924560861139,75.1121914622867,-11.9197708578082));
#10326=CARTESIAN_POINT('Ctrl Pts',(48.3995482155258,75.1123317029947,-12.0321911950802));
#10327=CARTESIAN_POINT('Ctrl Pts',(48.3907243897671,75.112157697847,-12.0874225881673));
#10328=CARTESIAN_POINT('Ctrl Pts',(48.3454843224248,75.111259785329,-12.2185054848428));
#10329=CARTESIAN_POINT('Ctrl Pts',(48.2991619954204,75.1103359104582,-12.2885292539931));
#10330=CARTESIAN_POINT('Ctrl Pts',(48.1374682888594,75.1070690230958,-12.4800885033658));
#10331=CARTESIAN_POINT('Ctrl Pts',(47.9801661690123,75.1038259424471,-12.5970480440319));
#10332=CARTESIAN_POINT('Ctrl Pts',(47.567931436684,75.0951655301064,-12.8514365775891));
#10333=CARTESIAN_POINT('Ctrl Pts',(47.2511618706613,75.088344063315,-12.9996046366577));
#10334=CARTESIAN_POINT('Ctrl Pts',(45.8398323679192,75.0589824950443,-13.5287651277848));
#10335=CARTESIAN_POINT('Ctrl Pts',(44.2829168047132,75.0275474210168,-13.8619012485751));
#10336=CARTESIAN_POINT('Ctrl Pts',(42.5,75.0275474210168,-13.8619012485751));
#10337=CARTESIAN_POINT('',(36.7497162970046,54.2657870626157,8.49707235020499));
#10338=CARTESIAN_POINT('Ctrl Pts',(42.5,56.4741768433204,8.41527182627157));
#10339=CARTESIAN_POINT('Ctrl Pts',(41.5425409623847,56.4741768433204,8.41527182627157));
#10340=CARTESIAN_POINT('Ctrl Pts',(40.5730846782016,56.3794041517534,8.42463245312286));
#10341=CARTESIAN_POINT('Ctrl Pts',(38.8128142163725,56.0096519365646,8.45306737297136));
#10342=CARTESIAN_POINT('Ctrl Pts',(38.1242861335929,55.7779082090862,8.46817771434433));
#10343=CARTESIAN_POINT('Ctrl Pts',(37.3990087340298,55.4395958991352,8.48356383163711));
#10344=CARTESIAN_POINT('Ctrl Pts',(37.1600081474467,55.3099988202737,8.48863432334797));
#10345=CARTESIAN_POINT('Ctrl Pts',(36.8756228074202,55.0919349938136,8.49451908749452));
#10346=CARTESIAN_POINT('Ctrl Pts',(36.7804309691012,55.0050263124736,8.49645752667339));
#10347=CARTESIAN_POINT('Ctrl Pts',(36.6725202371913,54.8557541081652,8.49862594939842));
#10348=CARTESIAN_POINT('Ctrl Pts',(36.6404757461974,54.7968898839877,8.49926313725424));
#10349=CARTESIAN_POINT('Ctrl Pts',(36.60578337376,54.6816671480108,8.4999510751473));
#10350=CARTESIAN_POINT('Ctrl Pts',(36.6000950949635,54.6284996690899,8.50006317420492));
#10351=CARTESIAN_POINT('Ctrl Pts',(36.6108031871309,54.5117737928708,8.4998514003521));
#10352=CARTESIAN_POINT('Ctrl Pts',(36.63095019812,54.4529115279528,8.49945311797868));
#10353=CARTESIAN_POINT('Ctrl Pts',(36.7054233466942,54.3105701888652,8.49796779174013));
#10354=CARTESIAN_POINT('Ctrl Pts',(36.7753659893159,54.2295066991348,8.49656158737708));
#10355=CARTESIAN_POINT('Ctrl Pts',(37.0105317420448,54.01386210121,8.49175055325143));
#10356=CARTESIAN_POINT('Ctrl Pts',(37.2098055238722,53.8921934273273,8.48756984405489));
#10357=CARTESIAN_POINT('Ctrl Pts',(37.7408106629893,53.6095844257818,8.47632459469298));
#10358=CARTESIAN_POINT('Ctrl Pts',(38.1963058893602,53.4296399345416,8.46644178421388));
#10359=CARTESIAN_POINT('Ctrl Pts',(40.1091410380517,52.8583430003522,8.42910834521598));
#10360=CARTESIAN_POINT('Ctrl Pts',(41.9765642728151,52.623608826244,8.40429614362558));
#10361=CARTESIAN_POINT('Ctrl Pts',(45.1609196154835,52.9459866017735,8.43254025942847));
#10362=CARTESIAN_POINT('Ctrl Pts',(46.1678099981393,53.2055054528039,8.45352083210801));
#10363=CARTESIAN_POINT('Ctrl Pts',(47.2697485955285,53.6201478825642,8.47646003133207));
#10364=CARTESIAN_POINT('Ctrl Pts',(47.5806825568242,53.7682807340069,8.48315877058117));
#10365=CARTESIAN_POINT('Ctrl Pts',(47.9620635928186,54.0043124559941,8.49116946879544));
#10366=CARTESIAN_POINT('Ctrl Pts',(48.1105225594668,54.112001721087,8.49424013684733));
#10367=CARTESIAN_POINT('Ctrl Pts',(48.2739688645561,54.2901330421496,8.49755420647477));
#10368=CARTESIAN_POINT('Ctrl Pts',(48.3224965288387,54.3563674241268,8.49852570518227));
#10369=CARTESIAN_POINT('Ctrl Pts',(48.3780029687332,54.4788517884074,8.49963039385909));
#10370=CARTESIAN_POINT('Ctrl Pts',(48.3924560861139,54.5320464525537,8.49991586754141));
#10371=CARTESIAN_POINT('Ctrl Pts',(48.3995482155258,54.6444667898256,8.50005610824948));
#10372=CARTESIAN_POINT('Ctrl Pts',(48.390724389767,54.6996981829127,8.49988210310169));
#10373=CARTESIAN_POINT('Ctrl Pts',(48.3454843224248,54.8307810795882,8.49898419058371));
#10374=CARTESIAN_POINT('Ctrl Pts',(48.2991619954204,54.9008048487383,8.498060315713));
#10375=CARTESIAN_POINT('Ctrl Pts',(48.13746828886,55.0923640981104,8.49479342835062));
#10376=CARTESIAN_POINT('Ctrl Pts',(47.9801661690137,55.2093236387763,8.49155034770193));
#10377=CARTESIAN_POINT('Ctrl Pts',(47.5679314366844,55.4637121723342,8.48288993536117));
#10378=CARTESIAN_POINT('Ctrl Pts',(47.251161870662,55.6118802314028,8.47606846856981));
#10379=CARTESIAN_POINT('Ctrl Pts',(45.8398323679184,56.1410407225304,8.4467069002991));
#10380=CARTESIAN_POINT('Ctrl Pts',(44.2829168047119,56.4741768433204,8.41527182627157));
#10381=CARTESIAN_POINT('Ctrl Pts',(42.5,56.4741768433204,8.41527182627157));
#10382=CARTESIAN_POINT('',(36.7497162970046,34.1152032445404,-12.3464885321295));
#10383=CARTESIAN_POINT('Ctrl Pts',(42.5,34.1970037684738,-10.1380987514247));
#10384=CARTESIAN_POINT('Ctrl Pts',(41.5425409623847,34.1970037684738,-10.1380987514247));
#10385=CARTESIAN_POINT('Ctrl Pts',(40.5730846782015,34.1876431416225,-10.2328714429918));
#10386=CARTESIAN_POINT('Ctrl Pts',(38.8128142163735,34.1592082217741,-10.6026236581803));
#10387=CARTESIAN_POINT('Ctrl Pts',(38.1242861335935,34.1440978804011,-10.8343673856586));
#10388=CARTESIAN_POINT('Ctrl Pts',(37.39900873403,34.1287117631083,-11.1726796956099));
#10389=CARTESIAN_POINT('Ctrl Pts',(37.1600081474469,34.1236412713974,-11.3022767744714));
#10390=CARTESIAN_POINT('Ctrl Pts',(36.8756228074203,34.1177565072509,-11.5203406009315));
#10391=CARTESIAN_POINT('Ctrl Pts',(36.7804309691013,34.115818068072,-11.6072492822715));
#10392=CARTESIAN_POINT('Ctrl Pts',(36.6725202371913,34.113649645347,-11.75652148658));
#10393=CARTESIAN_POINT('Ctrl Pts',(36.6404757461974,34.1130124574912,-11.8153857107575));
#10394=CARTESIAN_POINT('Ctrl Pts',(36.60578337376,34.1123245195981,-11.9306084467343));
#10395=CARTESIAN_POINT('Ctrl Pts',(36.6000950949635,34.1122124205405,-11.9837759256552));
#10396=CARTESIAN_POINT('Ctrl Pts',(36.6108031871309,34.1124241943933,-12.1005018018743));
#10397=CARTESIAN_POINT('Ctrl Pts',(36.63095019812,34.1128224767667,-12.1593640667924));
#10398=CARTESIAN_POINT('Ctrl Pts',(36.7054233466949,34.1143078030053,-12.3017054058813));
#10399=CARTESIAN_POINT('Ctrl Pts',(36.7753659893176,34.1157140073684,-12.3827688956119));
#10400=CARTESIAN_POINT('Ctrl Pts',(37.0105317420447,34.120525041494,-12.598413493535));
#10401=CARTESIAN_POINT('Ctrl Pts',(37.2098055238719,34.1247057506905,-12.7200821674178));
#10402=CARTESIAN_POINT('Ctrl Pts',(37.7408106629894,34.1359510000524,-13.0026911689634));
#10403=CARTESIAN_POINT('Ctrl Pts',(38.1963058893603,34.1458338105315,-13.1826356602036));
#10404=CARTESIAN_POINT('Ctrl Pts',(40.1091410380501,34.1831672495294,-13.7539325943925));
#10405=CARTESIAN_POINT('Ctrl Pts',(41.9765642728128,34.2079794511198,-13.9886667685015));
#10406=CARTESIAN_POINT('Ctrl Pts',(45.160919615482,34.1797353353169,-13.6662889929718));
#10407=CARTESIAN_POINT('Ctrl Pts',(46.1678099981384,34.1587547626374,-13.4067701419416));
#10408=CARTESIAN_POINT('Ctrl Pts',(47.2697485955313,34.1358155634133,-12.99212771218));
#10409=CARTESIAN_POINT('Ctrl Pts',(47.5806825568258,34.1291168241642,-12.8439948607373));
#10410=CARTESIAN_POINT('Ctrl Pts',(47.9620635928185,34.12110612595,-12.6079631387512));
#10411=CARTESIAN_POINT('Ctrl Pts',(48.1105225594667,34.1180354578981,-12.5002738736583));
#10412=CARTESIAN_POINT('Ctrl Pts',(48.273968864556,34.1147213882706,-12.3221425525957));
#10413=CARTESIAN_POINT('Ctrl Pts',(48.3224965288387,34.1137498895631,-12.2559081706184));
#10414=CARTESIAN_POINT('Ctrl Pts',(48.3780029687333,34.1126452008863,-12.1334238063378));
#10415=CARTESIAN_POINT('Ctrl Pts',(48.3924560861139,34.112359727204,-12.0802291421916));
#10416=CARTESIAN_POINT('Ctrl Pts',(48.3995482155258,34.1122194864959,-11.9678088049197));
#10417=CARTESIAN_POINT('Ctrl Pts',(48.3907243897671,34.1123934916437,-11.9125774118326));
#10418=CARTESIAN_POINT('Ctrl Pts',(48.3454843224248,34.1132914041617,-11.7814945151571));
#10419=CARTESIAN_POINT('Ctrl Pts',(48.2991619954205,34.1142152790324,-11.7114707460069));
#10420=CARTESIAN_POINT('Ctrl Pts',(48.1374682888603,34.1174821663948,-11.5199114966352));
#10421=CARTESIAN_POINT('Ctrl Pts',(47.9801661690144,34.1207252470435,-11.4029519559693));
#10422=CARTESIAN_POINT('Ctrl Pts',(47.5679314366847,34.1293856593842,-11.1485634224112));
#10423=CARTESIAN_POINT('Ctrl Pts',(47.2511618706624,34.1362071261756,-11.0003953633426));
#10424=CARTESIAN_POINT('Ctrl Pts',(45.8398323679199,34.1655686944463,-10.4712348722153));
#10425=CARTESIAN_POINT('Ctrl Pts',(44.2829168047143,34.1970037684738,-10.1380987514247));
#10426=CARTESIAN_POINT('Ctrl Pts',(42.5,34.1970037684738,-10.1380987514247));
#10427=CARTESIAN_POINT('Origin',(50.,54.6122755947453,-11.9999999999999));
#10428=CARTESIAN_POINT('',(50.,54.6122755947453,7.50000000000009));
#10429=CARTESIAN_POINT('Origin',(50.,54.6122755947453,-11.9999999999999));
#10430=CARTESIAN_POINT('Origin',(35.,54.6122755947453,-11.9999999999999));
#10431=CARTESIAN_POINT('',(35.,54.6122755947453,7.50000000000008));
#10432=CARTESIAN_POINT('Origin',(35.,54.6122755947453,-11.9999999999999));
#10433=CARTESIAN_POINT('',(35.,54.6122755947453,5.50000000000008));
#10434=CARTESIAN_POINT('Origin',(35.,54.6122755947453,-11.9999999999999));
#10435=CARTESIAN_POINT('Ctrl Pts',(36.6000954047721,75.6303323723191,-11.0710623055408));
#10436=CARTESIAN_POINT('Ctrl Pts',(36.6000954047721,75.1163129851934,-11.390036451076));
#10437=CARTESIAN_POINT('Ctrl Pts',(36.6000954047721,75.113533389205,-11.9949767040821));
#10438=CARTESIAN_POINT('Ctrl Pts',(36.6000954047721,75.1107537932165,-12.5999169570882));
#10439=CARTESIAN_POINT('Ctrl Pts',(36.6000954047721,75.6218202760576,-12.923601195162));
#10440=CARTESIAN_POINT('Ctrl Pts',(42.4997945641984,74.4160919611753,-9.11434223685902));
#10441=CARTESIAN_POINT('Ctrl Pts',(42.4997945641984,72.8193389779435,-10.1052054829035));
#10442=CARTESIAN_POINT('Ctrl Pts',(42.4997945641984,72.8107044238821,-11.9843956026886));
#10443=CARTESIAN_POINT('Ctrl Pts',(42.4997945641984,72.8020698698207,-13.8635857224736));
#10444=CARTESIAN_POINT('Ctrl Pts',(42.4997945641984,74.3896499330349,-14.8690804289273));
#10445=CARTESIAN_POINT('Ctrl Pts',(48.3995480441881,75.630258991695,-11.0709440543786));
#10446=CARTESIAN_POINT('Ctrl Pts',(48.3995480441881,75.1161741713435,-11.3899588044276));
#10447=CARTESIAN_POINT('Ctrl Pts',(48.3995480441881,75.1133942215203,-11.9949760646306));
#10448=CARTESIAN_POINT('Ctrl Pts',(48.3995480441881,75.1106142716971,-12.5999933248336));
#10449=CARTESIAN_POINT('Ctrl Pts',(48.3995480441881,75.6217458118676,-12.9237187670028));
#10450=CARTESIAN_POINT('Ctrl Pts',(36.6000954047721,53.6833379002862,9.01805677757378));
#10451=CARTESIAN_POINT('Ctrl Pts',(36.6000954047721,54.0023120458214,8.50403739044816));
#10452=CARTESIAN_POINT('Ctrl Pts',(36.6000954047721,54.6072522988275,8.50125779445973));
#10453=CARTESIAN_POINT('Ctrl Pts',(36.6000954047721,55.2121925518336,8.4984781984713));
#10454=CARTESIAN_POINT('Ctrl Pts',(36.6000954047721,55.5358767899073,9.00954468131236));
#10455=CARTESIAN_POINT('Ctrl Pts',(42.4997945641984,51.7266178316045,7.80381636642986));
#10456=CARTESIAN_POINT('Ctrl Pts',(42.4997945641984,52.7174810776491,6.2070633831982));
#10457=CARTESIAN_POINT('Ctrl Pts',(42.4997945641984,54.596671197434,6.19842882913689));
#10458=CARTESIAN_POINT('Ctrl Pts',(42.4997945641984,56.4758613172189,6.18979427507558));
#10459=CARTESIAN_POINT('Ctrl Pts',(42.4997945641984,57.4813560236726,7.77737433828968));
#10460=CARTESIAN_POINT('Ctrl Pts',(48.3995480441881,53.683219649124,9.0179833969497));
#10461=CARTESIAN_POINT('Ctrl Pts',(48.3995480441881,54.002234399173,8.50389857659829));
#10462=CARTESIAN_POINT('Ctrl Pts',(48.3995480441881,54.607251659376,8.50111862677509));
#10463=CARTESIAN_POINT('Ctrl Pts',(48.3995480441881,55.212268919579,8.49833867695189));
#10464=CARTESIAN_POINT('Ctrl Pts',(48.3995480441881,55.5359943617481,9.00947021712231));
#10465=CARTESIAN_POINT('Ctrl Pts',(36.6000954047722,33.5942188171715,-12.9289376944591));
#10466=CARTESIAN_POINT('Ctrl Pts',(36.6000954047722,34.1082382042972,-12.6099635489239));
#10467=CARTESIAN_POINT('Ctrl Pts',(36.6000954047722,34.1110178002857,-12.0050232959178));
#10468=CARTESIAN_POINT('Ctrl Pts',(36.6000954047722,34.1137973962741,-11.4000830429116));
#10469=CARTESIAN_POINT('Ctrl Pts',(36.6000954047722,33.602730913433,-11.0763988048379));
#10470=CARTESIAN_POINT('Ctrl Pts',(42.4997945641985,34.8084592283153,-14.8856577631409));
#10471=CARTESIAN_POINT('Ctrl Pts',(42.4997945641985,36.4052122115471,-13.8947945170964));
#10472=CARTESIAN_POINT('Ctrl Pts',(42.4997945641985,36.4138467656085,-12.0156043973113));
#10473=CARTESIAN_POINT('Ctrl Pts',(42.4997945641985,36.4224813196699,-10.1364142775263));
#10474=CARTESIAN_POINT('Ctrl Pts',(42.4997945641985,34.8349012564557,-9.13091957107256));
#10475=CARTESIAN_POINT('Ctrl Pts',(48.3995480441881,33.5942921977956,-12.9290559456212));
#10476=CARTESIAN_POINT('Ctrl Pts',(48.3995480441881,34.1083770181471,-12.6100411955723));
#10477=CARTESIAN_POINT('Ctrl Pts',(48.3995480441881,34.1111569679703,-12.0050239353692));
#10478=CARTESIAN_POINT('Ctrl Pts',(48.3995480441881,34.1139369177935,-11.4000066751662));
#10479=CARTESIAN_POINT('Ctrl Pts',(48.3995480441881,33.6028053776231,-11.0762812329971));
#10480=CARTESIAN_POINT('Ctrl Pts',(36.603289189263,55.5369296408085,-33.0088778576148));
#10481=CARTESIAN_POINT('Ctrl Pts',(36.603289189263,55.2128764217899,-32.4972287891192));
#10482=CARTESIAN_POINT('Ctrl Pts',(36.603289189263,54.6072465725666,-32.5000115536831));
#10483=CARTESIAN_POINT('Ctrl Pts',(36.603289189263,54.0016167233433,-32.5027943182471));
#10484=CARTESIAN_POINT('Ctrl Pts',(36.603289189263,53.682278966091,-33.0173996571641));
#10485=CARTESIAN_POINT('Ctrl Pts',(42.5,57.4802106040728,-31.7780997904234));
#10486=CARTESIAN_POINT('Ctrl Pts',(42.5,56.4751173200863,-30.1911535349279));
#10487=CARTESIAN_POINT('Ctrl Pts',(42.5,54.5966774271594,-30.1997846418264));
#10488=CARTESIAN_POINT('Ctrl Pts',(42.5,52.7182375342324,-30.2084157487249));
#10489=CARTESIAN_POINT('Ctrl Pts',(42.5,51.7277698693544,-31.8045312621439));
#10490=CARTESIAN_POINT('Ctrl Pts',(48.396710810737,55.5369296408085,-33.0088778576148));
#10491=CARTESIAN_POINT('Ctrl Pts',(48.396710810737,55.2128764217899,-32.4972287891192));
#10492=CARTESIAN_POINT('Ctrl Pts',(48.396710810737,54.6072465725666,-32.5000115536831));
#10493=CARTESIAN_POINT('Ctrl Pts',(48.396710810737,54.0016167233433,-32.5027943182471));
#10494=CARTESIAN_POINT('Ctrl Pts',(48.396710810737,53.682278966091,-33.0173996571641));
#10495=CARTESIAN_POINT('Origin',(47.5,69.4571012113211,2.84482561657582));
#10496=CARTESIAN_POINT('',(47.5,70.4387355541152,2.55242815321436));
#10497=CARTESIAN_POINT('',(47.5,69.1647037479597,3.82645995936986));
#10498=CARTESIAN_POINT('Origin',(47.5,69.4571012113211,2.84482561657582));
#10499=CARTESIAN_POINT('',(47.537899429919,70.3143910047143,2.28432898886365));
#10500=CARTESIAN_POINT('Ctrl Pts',(47.5,70.4387355541152,2.55242815321436));
#10501=CARTESIAN_POINT('Ctrl Pts',(47.5,70.4189527998948,2.48601365455714));
#10502=CARTESIAN_POINT('Ctrl Pts',(47.5053044417601,70.3925771182096,2.422112506851));
#10503=CARTESIAN_POINT('Ctrl Pts',(47.5230476022983,70.3458637388305,2.33479395638985));
#10504=CARTESIAN_POINT('Ctrl Pts',(47.5298073931343,70.3305302530218,2.30901426289197));
#10505=CARTESIAN_POINT('Ctrl Pts',(47.537899429919,70.3143910047143,2.28432898886365));
#10506=CARTESIAN_POINT('',(37.4621005700809,70.3143910047143,2.28432898886365));
#10507=CARTESIAN_POINT('',(47.537899429919,70.3143910047143,2.28432898886365));
#10508=CARTESIAN_POINT('',(37.5,70.4387355541152,2.55242815321436));
#10509=CARTESIAN_POINT('Ctrl Pts',(37.462100570081,70.3143910047143,2.28432898886366));
#10510=CARTESIAN_POINT('Ctrl Pts',(37.4632744099609,70.3167321820717,2.28790986224227));
#10511=CARTESIAN_POINT('Ctrl Pts',(37.4644207388779,70.3190574281895,2.29151535342116));
#10512=CARTESIAN_POINT('Ctrl Pts',(37.4898409184866,70.371513910436,2.37399296978792));
#10513=CARTESIAN_POINT('Ctrl Pts',(37.5,70.4113518729136,2.46049588543571));
#10514=CARTESIAN_POINT('Ctrl Pts',(37.5,70.4387355541152,2.55242815321435));
#10515=CARTESIAN_POINT('',(37.5,69.1647037479597,3.82645995936986));
#10516=CARTESIAN_POINT('Origin',(37.5,69.4571012113211,2.84482561657581));
#10517=CARTESIAN_POINT('',(37.4621005700809,68.8966045836089,3.70211540996904));
#10518=CARTESIAN_POINT('Ctrl Pts',(37.5,69.1647037479597,3.82645995936986));
#10519=CARTESIAN_POINT('Ctrl Pts',(37.5,69.0990912208333,3.80691608680946));
#10520=CARTESIAN_POINT('Ctrl Pts',(37.4948229521317,69.0359160073849,3.78093293985881));
#10521=CARTESIAN_POINT('Ctrl Pts',(37.4773121076774,68.948446705185,3.73440602894735));
#10522=CARTESIAN_POINT('Ctrl Pts',(37.470409170669,68.9219504993238,3.7186865862433));
#10523=CARTESIAN_POINT('Ctrl Pts',(37.462100570081,68.896604583609,3.70211540996904));
#10524=CARTESIAN_POINT('',(47.5378994299191,68.8966045836089,3.70211540996904));
#10525=CARTESIAN_POINT('',(47.5378994299191,68.8966045836089,3.70211540996904));
#10526=CARTESIAN_POINT('Ctrl Pts',(47.537899429919,68.8966045836089,3.70211540996903));
#10527=CARTESIAN_POINT('Ctrl Pts',(47.5369318666484,68.8995561970421,3.7040451767624));
#10528=CARTESIAN_POINT('Ctrl Pts',(47.5359829808858,68.9025245795757,3.7059641473824));
#10529=CARTESIAN_POINT('Ctrl Pts',(47.510332174293,68.9848409778267,3.75857431922063));
#10530=CARTESIAN_POINT('Ctrl Pts',(47.5,69.0719944289914,3.79884481948067));
#10531=CARTESIAN_POINT('Ctrl Pts',(47.5,69.1647037479597,3.82645995936986));
#10532=CARTESIAN_POINT('Origin',(47.5,54.6122755947453,-11.9999999999999));
#10533=CARTESIAN_POINT('Origin',(47.5,54.6122755947453,-11.9999999999999));
#10534=CARTESIAN_POINT('Origin',(37.5,54.6122755947453,-11.9999999999999));
#10535=CARTESIAN_POINT('Origin',(37.5,54.6122755947453,-11.9999999999999));
#10536=CARTESIAN_POINT('Origin',(47.5,68.349381898499,4.5391024665601));
#10537=CARTESIAN_POINT('Ctrl Pts',(37.4621005700809,68.896604583609,3.70211540996902));
#10538=CARTESIAN_POINT('Ctrl Pts',(37.4310083838403,68.8017558875511,3.6401032704416));
#10539=CARTESIAN_POINT('Ctrl Pts',(37.3828779782886,68.7018867262922,3.59772631179564));
#10540=CARTESIAN_POINT('Ctrl Pts',(37.245031822289,68.4694900791145,3.53679150015867));
#10541=CARTESIAN_POINT('Ctrl Pts',(37.1423703640038,68.3305669520952,3.52988534954539));
#10542=CARTESIAN_POINT('Ctrl Pts',(36.8667626334574,68.017493954875,3.57885731564907));
#10543=CARTESIAN_POINT('Ctrl Pts',(36.6872103879512,67.8515747651484,3.65364745765698));
#10544=CARTESIAN_POINT('Ctrl Pts',(36.5029780432796,67.7126857281249,3.76798632698662));
#10545=CARTESIAN_POINT('Ctrl Pts',(36.5014890205786,67.711565210995,3.76891288782061));
#10546=CARTESIAN_POINT('Ctrl Pts',(36.5,67.7104467215802,3.76984188672011));
#10547=CARTESIAN_POINT('Ctrl Pts',(47.537899429919,68.896604583609,3.70211540996901));
#10548=CARTESIAN_POINT('Ctrl Pts',(47.5689916161593,68.8017558875522,3.64010327044235));
#10549=CARTESIAN_POINT('Ctrl Pts',(47.6171220217102,68.7018867262946,3.59772631179665));
#10550=CARTESIAN_POINT('Ctrl Pts',(47.7549681777082,68.4694900791187,3.53679150015924));
#10551=CARTESIAN_POINT('Ctrl Pts',(47.8576296359926,68.3305669520998,3.52988534954533));
#10552=CARTESIAN_POINT('Ctrl Pts',(48.1332373665856,68.0174939548254,3.57885731565596));
#10553=CARTESIAN_POINT('Ctrl Pts',(48.3127896121225,67.8515747651177,3.65364745768193));
#10554=CARTESIAN_POINT('Ctrl Pts',(48.4970219567203,67.7126857281242,3.76798632698724));
#10555=CARTESIAN_POINT('Ctrl Pts',(48.498510979422,67.7115652109945,3.76891288782097));
#10556=CARTESIAN_POINT('Ctrl Pts',(48.5,67.7104467215802,3.7698418867201));
#10557=CARTESIAN_POINT('Origin',(48.5,54.6122755947453,-11.9999999999999));
#10558=CARTESIAN_POINT('Ctrl Pts',(47.537899429919,70.3143910047143,2.28432898886365));
#10559=CARTESIAN_POINT('Ctrl Pts',(47.5689916161588,70.2523788651886,2.18948029280836));
#10560=CARTESIAN_POINT('Ctrl Pts',(47.6171220217088,70.2100019065432,2.08961113155225));
#10561=CARTESIAN_POINT('Ctrl Pts',(47.7549681777051,70.1490670949051,1.85721448437786));
#10562=CARTESIAN_POINT('Ctrl Pts',(47.8576296359887,70.1421609442907,1.71829135735951));
#10563=CARTESIAN_POINT('Ctrl Pts',(48.1332373666213,70.1911329104067,1.40521836003877));
#10564=CARTESIAN_POINT('Ctrl Pts',(48.3127896121854,70.2659230524474,1.23929917034817));
#10565=CARTESIAN_POINT('Ctrl Pts',(48.4970219567186,70.3802619217321,1.10041013337938));
#10566=CARTESIAN_POINT('Ctrl Pts',(48.4985109794219,70.3811884825662,1.09928961624927));
#10567=CARTESIAN_POINT('Ctrl Pts',(48.5,70.3821174814654,1.09817112683487));
#10568=CARTESIAN_POINT('Origin',(36.5,54.6122755947453,-11.9999999999999));
#10569=CARTESIAN_POINT('Ctrl Pts',(37.4621005700809,70.3143910047143,2.28432898886365));
#10570=CARTESIAN_POINT('Ctrl Pts',(37.4310083838412,70.2523788651887,2.18948029280845));
#10571=CARTESIAN_POINT('Ctrl Pts',(37.3828779782913,70.2100019065433,2.08961113155242));
#10572=CARTESIAN_POINT('Ctrl Pts',(37.2450318222954,70.1490670949052,1.85721448437858));
#10573=CARTESIAN_POINT('Ctrl Pts',(37.1423703640119,70.1421609442906,1.71829135736027));
#10574=CARTESIAN_POINT('Ctrl Pts',(36.8667626333773,70.1911329104068,1.40521836003708));
#10575=CARTESIAN_POINT('Ctrl Pts',(36.6872103878129,70.2659230524489,1.23929917034637));
#10576=CARTESIAN_POINT('Ctrl Pts',(36.5029780432807,70.3802619217326,1.10041013337885));
#10577=CARTESIAN_POINT('Ctrl Pts',(36.5014890205792,70.3811884825656,1.09928961625003));
#10578=CARTESIAN_POINT('Ctrl Pts',(36.5,70.3821174814654,1.09817112683487));
#10579=CARTESIAN_POINT('Origin',(50.,71.1513780613054,1.73710630375365));
#10580=CARTESIAN_POINT('Origin',(47.5,39.7674499781698,2.84482561657604));
#10581=CARTESIAN_POINT('',(47.5,40.0598474415312,3.82645995937007));
#10582=CARTESIAN_POINT('',(47.5,38.7858156353757,2.5524281532146));
#10583=CARTESIAN_POINT('Origin',(47.5,39.7674499781698,2.84482561657604));
#10584=CARTESIAN_POINT('',(47.5378994299191,40.3279466058819,3.70211540996925));
#10585=CARTESIAN_POINT('Ctrl Pts',(47.5,40.0598474415312,3.82645995937007));
#10586=CARTESIAN_POINT('Ctrl Pts',(47.5,40.1262619401886,3.80667720514962));
#10587=CARTESIAN_POINT('Ctrl Pts',(47.5053044417602,40.1901630878949,3.7803015234644));
#10588=CARTESIAN_POINT('Ctrl Pts',(47.5230476022984,40.277481638356,3.73358814408523));
#10589=CARTESIAN_POINT('Ctrl Pts',(47.5298073931343,40.3032613318537,3.71825465827663));
#10590=CARTESIAN_POINT('Ctrl Pts',(47.537899429919,40.3279466058819,3.70211540996925));
#10591=CARTESIAN_POINT('',(37.462100570081,40.3279466058819,3.70211540996925));
#10592=CARTESIAN_POINT('',(47.5378994299191,40.3279466058819,3.70211540996925));
#10593=CARTESIAN_POINT('',(37.5,40.0598474415312,3.82645995937007));
#10594=CARTESIAN_POINT('Ctrl Pts',(37.462100570081,40.3279466058819,3.70211540996925));
#10595=CARTESIAN_POINT('Ctrl Pts',(37.4632744099609,40.3243657325033,3.70445658732663));
#10596=CARTESIAN_POINT('Ctrl Pts',(37.4644207388779,40.3207602413243,3.70678183344449));
#10597=CARTESIAN_POINT('Ctrl Pts',(37.4898409184866,40.2382826249574,3.75923831569102));
#10598=CARTESIAN_POINT('Ctrl Pts',(37.5,40.1517797093097,3.7990762781686));
#10599=CARTESIAN_POINT('Ctrl Pts',(37.5,40.0598474415312,3.82645995937007));
#10600=CARTESIAN_POINT('',(37.5,38.7858156353757,2.55242815321459));
#10601=CARTESIAN_POINT('Origin',(37.5,39.7674499781698,2.84482561657603));
#10602=CARTESIAN_POINT('',(37.462100570081,38.9101601847765,2.28432898886388));
#10603=CARTESIAN_POINT('Ctrl Pts',(37.5,38.7858156353757,2.55242815321459));
#10604=CARTESIAN_POINT('Ctrl Pts',(37.5,38.8053595079361,2.48681562608814));
#10605=CARTESIAN_POINT('Ctrl Pts',(37.4948229521316,38.8313426548868,2.42364041263967));
#10606=CARTESIAN_POINT('Ctrl Pts',(37.4773121076774,38.8778695657982,2.33617111043986));
#10607=CARTESIAN_POINT('Ctrl Pts',(37.470409170669,38.8935890085023,2.3096749045787));
#10608=CARTESIAN_POINT('Ctrl Pts',(37.462100570081,38.9101601847765,2.28432898886388));
#10609=CARTESIAN_POINT('',(47.5378994299191,38.9101601847765,2.28432898886388));
#10610=CARTESIAN_POINT('',(47.5378994299191,38.9101601847765,2.28432898886388));
#10611=CARTESIAN_POINT('Ctrl Pts',(47.537899429919,38.9101601847765,2.28432898886389));
#10612=CARTESIAN_POINT('Ctrl Pts',(47.5369318666484,38.9082304179831,2.28728060229702));
#10613=CARTESIAN_POINT('Ctrl Pts',(47.5359829808858,38.9063114473632,2.29024898483066));
#10614=CARTESIAN_POINT('Ctrl Pts',(47.5103321742929,38.8537012755249,2.37256538308168));
#10615=CARTESIAN_POINT('Ctrl Pts',(47.5,38.8134307752649,2.45971883424642));
#10616=CARTESIAN_POINT('Ctrl Pts',(47.5,38.7858156353757,2.5524281532146));
#10617=CARTESIAN_POINT('Origin',(47.5,54.6122755947453,-11.9999999999999));
#10618=CARTESIAN_POINT('Origin',(47.5,54.6122755947453,-11.9999999999999));
#10619=CARTESIAN_POINT('Origin',(37.5,54.6122755947453,-11.9999999999999));
#10620=CARTESIAN_POINT('Origin',(37.5,54.6122755947453,-11.9999999999999));
#10621=CARTESIAN_POINT('Origin',(47.5,39.7674499781695,-26.8448256165756));
#10622=CARTESIAN_POINT('',(47.5,38.7858156353755,-26.5524281532142));
#10623=CARTESIAN_POINT('',(47.5,40.059847441531,-27.8264599593697));
#10624=CARTESIAN_POINT('Origin',(47.5,39.7674499781695,-26.8448256165756));
#10625=CARTESIAN_POINT('',(47.5378994299191,38.9101601847763,-26.2843289888635));
#10626=CARTESIAN_POINT('Ctrl Pts',(47.5,38.7858156353755,-26.5524281532142));
#10627=CARTESIAN_POINT('Ctrl Pts',(47.5,38.8055983895958,-26.4860136545571));
#10628=CARTESIAN_POINT('Ctrl Pts',(47.5053044417601,38.8319740712809,-26.4221125068513));
#10629=CARTESIAN_POINT('Ctrl Pts',(47.5230476022982,38.8786874506599,-26.3347939563902));
#10630=CARTESIAN_POINT('Ctrl Pts',(47.5298073931342,38.8940209364687,-26.309014262892));
#10631=CARTESIAN_POINT('Ctrl Pts',(47.5378994299191,38.9101601847763,-26.2843289888635));
#10632=CARTESIAN_POINT('',(37.462100570081,38.9101601847763,-26.2843289888635));
#10633=CARTESIAN_POINT('',(47.5378994299191,38.9101601847763,-26.2843289888635));
#10634=CARTESIAN_POINT('',(37.5,38.7858156353755,-26.5524281532142));
#10635=CARTESIAN_POINT('Ctrl Pts',(37.462100570081,38.9101601847763,-26.2843289888635));
#10636=CARTESIAN_POINT('Ctrl Pts',(37.463274409961,38.9078190074188,-26.2879098622423));
#10637=CARTESIAN_POINT('Ctrl Pts',(37.464420738878,38.9054937613009,-26.2915153534214));
#10638=CARTESIAN_POINT('Ctrl Pts',(37.4898409184867,38.8530372790542,-26.3739929697886));
#10639=CARTESIAN_POINT('Ctrl Pts',(37.5,38.8131993165768,-26.4604958854362));
#10640=CARTESIAN_POINT('Ctrl Pts',(37.5,38.7858156353755,-26.5524281532142));
#10641=CARTESIAN_POINT('',(37.5,40.059847441531,-27.8264599593697));
#10642=CARTESIAN_POINT('Origin',(37.5,39.7674499781695,-26.8448256165756));
#10643=CARTESIAN_POINT('',(37.462100570081,40.3279466058817,-27.7021154099689));
#10644=CARTESIAN_POINT('Ctrl Pts',(37.5,40.059847441531,-27.8264599593697));
#10645=CARTESIAN_POINT('Ctrl Pts',(37.5,40.1254599686575,-27.8069160868092));
#10646=CARTESIAN_POINT('Ctrl Pts',(37.4948229521316,40.1886351821059,-27.7809329398586));
#10647=CARTESIAN_POINT('Ctrl Pts',(37.4773121076774,40.2761044843057,-27.7344060289472));
#10648=CARTESIAN_POINT('Ctrl Pts',(37.470409170669,40.3026006901669,-27.7186865862431));
#10649=CARTESIAN_POINT('Ctrl Pts',(37.462100570081,40.3279466058817,-27.7021154099689));
#10650=CARTESIAN_POINT('',(47.5378994299191,40.3279466058817,-27.7021154099689));
#10651=CARTESIAN_POINT('',(47.5378994299191,40.3279466058817,-27.7021154099689));
#10652=CARTESIAN_POINT('Ctrl Pts',(47.5378994299191,40.3279466058817,-27.7021154099689));
#10653=CARTESIAN_POINT('Ctrl Pts',(47.5369318666484,40.3249949924486,-27.7040451767622));
#10654=CARTESIAN_POINT('Ctrl Pts',(47.5359829808858,40.3220266099149,-27.7059641473822));
#10655=CARTESIAN_POINT('Ctrl Pts',(47.5103321742929,40.2397102116637,-27.7585743192207));
#10656=CARTESIAN_POINT('Ctrl Pts',(47.5,40.1525567604989,-27.7988448194806));
#10657=CARTESIAN_POINT('Ctrl Pts',(47.5,40.059847441531,-27.8264599593697));
#10658=CARTESIAN_POINT('Origin',(47.5,54.6122755947453,-11.9999999999999));
#10659=CARTESIAN_POINT('Origin',(47.5,54.6122755947453,-11.9999999999999));
#10660=CARTESIAN_POINT('Origin',(37.5,54.6122755947453,-11.9999999999999));
#10661=CARTESIAN_POINT('Origin',(37.5,54.6122755947453,-11.9999999999999));
#10662=CARTESIAN_POINT('Origin',(47.5,69.457101211321,-26.8448256165758));
#10663=CARTESIAN_POINT('',(47.5,69.1647037479595,-27.8264599593698));
#10664=CARTESIAN_POINT('',(47.5,70.4387355541151,-26.5524281532143));
#10665=CARTESIAN_POINT('Origin',(47.5,69.457101211321,-26.8448256165758));
#10666=CARTESIAN_POINT('',(47.5378994299191,68.8966045836088,-27.702115409969));
#10667=CARTESIAN_POINT('Ctrl Pts',(47.5,69.1647037479595,-27.8264599593698));
#10668=CARTESIAN_POINT('Ctrl Pts',(47.5,69.0982892493024,-27.8066772051495));
#10669=CARTESIAN_POINT('Ctrl Pts',(47.5053044417601,69.0343881015963,-27.7803015234644));
#10670=CARTESIAN_POINT('Ctrl Pts',(47.5230476022983,68.9470695511352,-27.7335881440852));
#10671=CARTESIAN_POINT('Ctrl Pts',(47.5298073931342,68.9212898576372,-27.7182546582765));
#10672=CARTESIAN_POINT('Ctrl Pts',(47.5378994299191,68.8966045836088,-27.702115409969));
#10673=CARTESIAN_POINT('',(37.462100570081,68.8966045836088,-27.702115409969));
#10674=CARTESIAN_POINT('',(47.5378994299191,68.8966045836088,-27.702115409969));
#10675=CARTESIAN_POINT('',(37.5,69.1647037479595,-27.8264599593698));
#10676=CARTESIAN_POINT('Ctrl Pts',(37.462100570081,68.8966045836088,-27.702115409969));
#10677=CARTESIAN_POINT('Ctrl Pts',(37.4632744099607,68.900185456987,-27.704456587326));
#10678=CARTESIAN_POINT('Ctrl Pts',(37.4644207388776,68.9037909481654,-27.7067818334436));
#10679=CARTESIAN_POINT('Ctrl Pts',(37.4898409184865,68.9862685645324,-27.7592383156903));
#10680=CARTESIAN_POINT('Ctrl Pts',(37.5,69.0727714801806,-27.7990762781682));
#10681=CARTESIAN_POINT('Ctrl Pts',(37.5,69.1647037479595,-27.8264599593698));
#10682=CARTESIAN_POINT('',(37.5,70.4387355541151,-26.5524281532143));
#10683=CARTESIAN_POINT('Origin',(37.5,69.457101211321,-26.8448256165758));
#10684=CARTESIAN_POINT('',(37.462100570081,70.3143910047142,-26.2843289888636));
#10685=CARTESIAN_POINT('Ctrl Pts',(37.5,70.4387355541151,-26.5524281532143));
#10686=CARTESIAN_POINT('Ctrl Pts',(37.5,70.4191916815546,-26.4868156260878));
#10687=CARTESIAN_POINT('Ctrl Pts',(37.4948229521316,70.3932085346039,-26.4236404126394));
#10688=CARTESIAN_POINT('Ctrl Pts',(37.4773121076774,70.3466816236925,-26.3361711104396));
#10689=CARTESIAN_POINT('Ctrl Pts',(37.470409170669,70.3309621809885,-26.3096749045784));
#10690=CARTESIAN_POINT('Ctrl Pts',(37.462100570081,70.3143910047142,-26.2843289888636));
#10691=CARTESIAN_POINT('',(47.5378994299191,70.3143910047142,-26.2843289888636));
#10692=CARTESIAN_POINT('',(47.5378994299191,70.3143910047142,-26.2843289888636));
#10693=CARTESIAN_POINT('Ctrl Pts',(47.5378994299191,70.3143910047142,-26.2843289888636));
#10694=CARTESIAN_POINT('Ctrl Pts',(47.5369318666484,70.3163207715076,-26.2872806022967));
#10695=CARTESIAN_POINT('Ctrl Pts',(47.5359829808858,70.3182397421275,-26.2902489848303));
#10696=CARTESIAN_POINT('Ctrl Pts',(47.510332174293,70.3708499139657,-26.3725653830812));
#10697=CARTESIAN_POINT('Ctrl Pts',(47.5,70.4111204142258,-26.4597188342459));
#10698=CARTESIAN_POINT('Ctrl Pts',(47.5,70.4387355541151,-26.5524281532143));
#10699=CARTESIAN_POINT('Origin',(47.5,54.6122755947453,-11.9999999999999));
#10700=CARTESIAN_POINT('Origin',(47.5,54.6122755947453,-11.9999999999999));
#10701=CARTESIAN_POINT('Origin',(37.5,54.6122755947453,-11.9999999999999));
#10702=CARTESIAN_POINT('Origin',(37.5,54.6122755947453,-11.9999999999999));
#10703=CARTESIAN_POINT('Origin',(47.5,71.1513780613053,-25.7371063037536));
#10704=CARTESIAN_POINT('Ctrl Pts',(37.462100570081,70.3143910047142,-26.2843289888636));
#10705=CARTESIAN_POINT('Ctrl Pts',(37.4310083838417,70.2523788651895,-26.1894802928099));
#10706=CARTESIAN_POINT('Ctrl Pts',(37.3828779782928,70.2100019065445,-26.0896111315555));
#10707=CARTESIAN_POINT('Ctrl Pts',(37.2450318222992,70.1490670949059,-25.8572144843843));
#10708=CARTESIAN_POINT('Ctrl Pts',(37.1423703640169,70.1421609442904,-25.7182913573665));
#10709=CARTESIAN_POINT('Ctrl Pts',(36.8667626333183,70.1911329104162,-25.4052183599692));
#10710=CARTESIAN_POINT('Ctrl Pts',(36.6872103877121,70.2659230524829,-25.2392991703043));
#10711=CARTESIAN_POINT('Ctrl Pts',(36.5029780432812,70.3802619217331,-25.1004101333781));
#10712=CARTESIAN_POINT('Ctrl Pts',(36.5014890205775,70.3811884825665,-25.0992896162488));
#10713=CARTESIAN_POINT('Ctrl Pts',(36.5,70.3821174814653,-25.0981711268349));
#10714=CARTESIAN_POINT('Ctrl Pts',(47.5378994299191,70.3143910047142,-26.2843289888636));
#10715=CARTESIAN_POINT('Ctrl Pts',(47.568991616158,70.2523788651901,-26.1894802928108));
#10716=CARTESIAN_POINT('Ctrl Pts',(47.6171220217063,70.2100019065453,-26.0896111315574));
#10717=CARTESIAN_POINT('Ctrl Pts',(47.7549681776988,70.1490670949063,-25.8572144843871));
#10718=CARTESIAN_POINT('Ctrl Pts',(47.8576296359807,70.1421609442904,-25.7182913573697));
#10719=CARTESIAN_POINT('Ctrl Pts',(48.1332373667109,70.1911329104208,-25.4052183599355));
#10720=CARTESIAN_POINT('Ctrl Pts',(48.3127896123394,70.2659230524989,-25.2392991702846));
#10721=CARTESIAN_POINT('Ctrl Pts',(48.4970219567185,70.3802619217334,-25.1004101333777));
#10722=CARTESIAN_POINT('Ctrl Pts',(48.4985109794227,70.3811884825666,-25.0992896162486));
#10723=CARTESIAN_POINT('Ctrl Pts',(48.5,70.3821174814653,-25.0981711268349));
#10724=CARTESIAN_POINT('Origin',(48.5,54.6122755947453,-11.9999999999999));
#10725=CARTESIAN_POINT('Ctrl Pts',(47.5378994299191,68.8966045836088,-27.702115409969));
#10726=CARTESIAN_POINT('Ctrl Pts',(47.5689916161593,68.8017558875521,-27.6401032704423));
#10727=CARTESIAN_POINT('Ctrl Pts',(47.6171220217102,68.7018867262945,-27.5977263117966));
#10728=CARTESIAN_POINT('Ctrl Pts',(47.7549681777078,68.4694900791192,-27.5367915001594));
#10729=CARTESIAN_POINT('Ctrl Pts',(47.857629635992,68.3305669521004,-27.5298853495452));
#10730=CARTESIAN_POINT('Ctrl Pts',(48.1332373665661,68.0174939548474,-27.5788573156524));
#10731=CARTESIAN_POINT('Ctrl Pts',(48.3127896120915,67.8515747651331,-27.6536474576698));
#10732=CARTESIAN_POINT('Ctrl Pts',(48.4970219567174,67.7126857281265,-27.7679863269852));
#10733=CARTESIAN_POINT('Ctrl Pts',(48.4985109794222,67.7115652109942,-27.7689128878211));
#10734=CARTESIAN_POINT('Ctrl Pts',(48.5,67.71044672158,-27.7698418867201));
#10735=CARTESIAN_POINT('Origin',(36.5,54.6122755947453,-11.9999999999999));
#10736=CARTESIAN_POINT('Ctrl Pts',(37.462100570081,68.8966045836088,-27.702115409969));
#10737=CARTESIAN_POINT('Ctrl Pts',(37.4310083838413,68.8017558875538,-27.6401032704434));
#10738=CARTESIAN_POINT('Ctrl Pts',(37.3828779782915,68.701886726298,-27.5977263117981));
#10739=CARTESIAN_POINT('Ctrl Pts',(37.245031822296,68.4694900791247,-27.5367915001601));
#10740=CARTESIAN_POINT('Ctrl Pts',(37.1423703640128,68.3305669521065,-27.5298853495452));
#10741=CARTESIAN_POINT('Ctrl Pts',(36.8667626333661,68.0174939547694,-27.5788573156634));
#10742=CARTESIAN_POINT('Ctrl Pts',(36.6872103877933,67.8515747650841,-27.6536474577095));
#10743=CARTESIAN_POINT('Ctrl Pts',(36.5029780432822,67.7126857281249,-27.7679863269865));
#10744=CARTESIAN_POINT('Ctrl Pts',(36.5014890205769,67.7115652109935,-27.7689128878217));
#10745=CARTESIAN_POINT('Ctrl Pts',(36.5,67.71044672158,-27.7698418867201));
#10746=CARTESIAN_POINT('Origin',(50.,68.3493818984988,-28.5391024665601));
#10747=CARTESIAN_POINT('Origin',(47.5,40.8751692909917,-28.5391024665599));
#10748=CARTESIAN_POINT('Ctrl Pts',(37.462100570081,40.3279466058817,-27.7021154099689));
#10749=CARTESIAN_POINT('Ctrl Pts',(37.4310083838416,40.4227953019356,-27.640103270444));
#10750=CARTESIAN_POINT('Ctrl Pts',(37.3828779782926,40.5226644631903,-27.5977263117989));
#10751=CARTESIAN_POINT('Ctrl Pts',(37.2450318222986,40.755061110362,-27.5367915001605));
#10752=CARTESIAN_POINT('Ctrl Pts',(37.1423703640161,40.8939842373798,-27.529885349545));
#10753=CARTESIAN_POINT('Ctrl Pts',(36.8667626333263,41.2070572347668,-27.5788573156696));
#10754=CARTESIAN_POINT('Ctrl Pts',(36.6872103877253,41.3729764244348,-27.6536474577325));
#10755=CARTESIAN_POINT('Ctrl Pts',(36.5029780432813,41.511865461367,-27.7679863269875));
#10756=CARTESIAN_POINT('Ctrl Pts',(36.5014890205774,41.5129859784966,-27.7689128878212));
#10757=CARTESIAN_POINT('Ctrl Pts',(36.5,41.5141044679104,-27.7698418867199));
#10758=CARTESIAN_POINT('Ctrl Pts',(47.5378994299191,40.3279466058817,-27.7021154099689));
#10759=CARTESIAN_POINT('Ctrl Pts',(47.5689916161584,40.4227953019356,-27.640103270444));
#10760=CARTESIAN_POINT('Ctrl Pts',(47.6171220217074,40.5226644631902,-27.597726311799));
#10761=CARTESIAN_POINT('Ctrl Pts',(47.7549681777013,40.7550611103619,-27.5367915001605));
#10762=CARTESIAN_POINT('Ctrl Pts',(47.8576296359839,40.8939842373797,-27.5298853495451));
#10763=CARTESIAN_POINT('Ctrl Pts',(48.1332373666762,41.2070572347697,-27.57885731567));
#10764=CARTESIAN_POINT('Ctrl Pts',(48.3127896122781,41.3729764244373,-27.6536474577346));
#10765=CARTESIAN_POINT('Ctrl Pts',(48.497021956718,41.5118654613665,-27.7679863269871));
#10766=CARTESIAN_POINT('Ctrl Pts',(48.4985109794233,41.5129859784971,-27.7689128878216));
#10767=CARTESIAN_POINT('Ctrl Pts',(48.5,41.5141044679105,-27.7698418867199));
#10768=CARTESIAN_POINT('Origin',(48.5,54.6122755947453,-11.9999999999999));
#10769=CARTESIAN_POINT('Ctrl Pts',(47.5378994299191,38.9101601847763,-26.2843289888635));
#10770=CARTESIAN_POINT('Ctrl Pts',(47.5689916161584,38.9721723243012,-26.1894802928096));
#10771=CARTESIAN_POINT('Ctrl Pts',(47.6171220217074,39.0145492829462,-26.0896111315549));
#10772=CARTESIAN_POINT('Ctrl Pts',(47.7549681777013,39.0754840945847,-25.8572144843834));
#10773=CARTESIAN_POINT('Ctrl Pts',(47.8576296359838,39.0823902452002,-25.7182913573655));
#10774=CARTESIAN_POINT('Ctrl Pts',(48.1332373666738,39.0334182790756,-25.4052183599782));
#10775=CARTESIAN_POINT('Ctrl Pts',(48.3127896122749,38.9586281370126,-25.2392991703103));
#10776=CARTESIAN_POINT('Ctrl Pts',(48.497021956719,38.8442892677574,-25.1004101333779));
#10777=CARTESIAN_POINT('Ctrl Pts',(48.4985109794223,38.8433627069242,-25.0992896162488));
#10778=CARTESIAN_POINT('Ctrl Pts',(48.5,38.8424337080252,-25.0981711268347));
#10779=CARTESIAN_POINT('Origin',(36.5,54.6122755947453,-11.9999999999999));
#10780=CARTESIAN_POINT('Ctrl Pts',(37.462100570081,38.9101601847763,-26.2843289888635));
#10781=CARTESIAN_POINT('Ctrl Pts',(37.4310083838421,38.9721723243003,-26.1894802928109));
#10782=CARTESIAN_POINT('Ctrl Pts',(37.3828779782939,39.0145492829451,-26.0896111315576));
#10783=CARTESIAN_POINT('Ctrl Pts',(37.2450318223019,39.075484094584,-25.8572144843881));
#10784=CARTESIAN_POINT('Ctrl Pts',(37.1423703640203,39.0823902452002,-25.7182913573708));
#10785=CARTESIAN_POINT('Ctrl Pts',(36.8667626332853,39.0334182790692,-25.4052183599309));
#10786=CARTESIAN_POINT('Ctrl Pts',(36.6872103876556,38.9586281369882,-25.2392991702806));
#10787=CARTESIAN_POINT('Ctrl Pts',(36.502978043283,38.844289267758,-25.1004101333787));
#10788=CARTESIAN_POINT('Ctrl Pts',(36.5014890205765,38.8433627069234,-25.0992896162479));
#10789=CARTESIAN_POINT('Ctrl Pts',(36.5,38.8424337080252,-25.0981711268347));
#10790=CARTESIAN_POINT('Origin',(50.,38.0731731281852,-25.7371063037535));
#10791=CARTESIAN_POINT('Origin',(47.5,38.0731731281855,1.73710630375391));
#10792=CARTESIAN_POINT('Ctrl Pts',(37.462100570081,38.9101601847765,2.2843289888639));
#10793=CARTESIAN_POINT('Ctrl Pts',(37.4310083838418,38.9721723243011,2.1894802928104));
#10794=CARTESIAN_POINT('Ctrl Pts',(37.382877978293,39.0145492829461,2.0896111315562));
#10795=CARTESIAN_POINT('Ctrl Pts',(37.2450318222997,39.0754840945847,1.85721448438531));
#10796=CARTESIAN_POINT('Ctrl Pts',(37.1423703640175,39.0823902452004,1.71829135736766));
#10797=CARTESIAN_POINT('Ctrl Pts',(36.8667626333158,39.0334182790742,1.40521835996645));
#10798=CARTESIAN_POINT('Ctrl Pts',(36.6872103877081,38.9586281370059,1.23929917030242));
#10799=CARTESIAN_POINT('Ctrl Pts',(36.5029780432818,38.844289267758,1.10041013337881));
#10800=CARTESIAN_POINT('Ctrl Pts',(36.5014890205776,38.8433627069243,1.09928961624914));
#10801=CARTESIAN_POINT('Ctrl Pts',(36.5,38.8424337080254,1.09817112683512));
#10802=CARTESIAN_POINT('Ctrl Pts',(47.5378994299191,38.9101601847765,2.2843289888639));
#10803=CARTESIAN_POINT('Ctrl Pts',(47.5689916161585,38.9721723243016,2.18948029280961));
#10804=CARTESIAN_POINT('Ctrl Pts',(47.6171220217078,39.0145492829468,2.08961113155459));
#10805=CARTESIAN_POINT('Ctrl Pts',(47.7549681777024,39.0754840945851,1.85721448438222));
#10806=CARTESIAN_POINT('Ctrl Pts',(47.8576296359852,39.0823902452003,1.71829135736426));
#10807=CARTESIAN_POINT('Ctrl Pts',(48.1332373666565,39.0334182790786,1.40521835999846));
#10808=CARTESIAN_POINT('Ctrl Pts',(48.3127896122453,38.9586281370227,1.23929917032299));
#10809=CARTESIAN_POINT('Ctrl Pts',(48.4970219567186,38.8442892677582,1.10041013337901));
#10810=CARTESIAN_POINT('Ctrl Pts',(48.4985109794219,38.8433627069246,1.09928961624948));
#10811=CARTESIAN_POINT('Ctrl Pts',(48.5,38.8424337080254,1.09817112683513));
#10812=CARTESIAN_POINT('Origin',(48.5,54.6122755947453,-11.9999999999999));
#10813=CARTESIAN_POINT('Ctrl Pts',(47.5378994299191,40.3279466058819,3.70211540996925));
#10814=CARTESIAN_POINT('Ctrl Pts',(47.5689916161576,40.4227953019335,3.64010327044594));
#10815=CARTESIAN_POINT('Ctrl Pts',(47.6171220217051,40.5226644631856,3.59772631180138));
#10816=CARTESIAN_POINT('Ctrl Pts',(47.7549681776959,40.7550611103542,3.53679150016188));
#10817=CARTESIAN_POINT('Ctrl Pts',(47.857629635977,40.8939842373711,3.5298853495454));
#10818=CARTESIAN_POINT('Ctrl Pts',(48.1332373667501,41.2070572348553,3.57885731568198));
#10819=CARTESIAN_POINT('Ctrl Pts',(48.3127896124051,41.3729764244901,3.65364745777795));
#10820=CARTESIAN_POINT('Ctrl Pts',(48.4970219567172,41.5118654613675,3.76798632698816));
#10821=CARTESIAN_POINT('Ctrl Pts',(48.4985109794234,41.5129859784975,3.76891288782207));
#10822=CARTESIAN_POINT('Ctrl Pts',(48.5,41.5141044679107,3.76984188672031));
#10823=CARTESIAN_POINT('Origin',(36.5,54.6122755947453,-11.9999999999999));
#10824=CARTESIAN_POINT('Ctrl Pts',(37.462100570081,40.3279466058819,3.70211540996925));
#10825=CARTESIAN_POINT('Ctrl Pts',(37.4310083838421,40.4227953019343,3.64010327044543));
#10826=CARTESIAN_POINT('Ctrl Pts',(37.3828779782942,40.5226644631872,3.5977263118007));
#10827=CARTESIAN_POINT('Ctrl Pts',(37.2450318223022,40.755061110357,3.53679150016149));
#10828=CARTESIAN_POINT('Ctrl Pts',(37.1423703640206,40.8939842373742,3.52988534954544));
#10829=CARTESIAN_POINT('Ctrl Pts',(36.8667626332747,41.2070572348267,3.57885731567809));
#10830=CARTESIAN_POINT('Ctrl Pts',(36.6872103876371,41.3729764244722,3.65364745776331));
#10831=CARTESIAN_POINT('Ctrl Pts',(36.5029780432816,41.511865461368,3.76798632698854));
#10832=CARTESIAN_POINT('Ctrl Pts',(36.5014890205776,41.5129859784967,3.76891288782145));
#10833=CARTESIAN_POINT('Ctrl Pts',(36.5,41.5141044679107,3.76984188672031));
#10834=CARTESIAN_POINT('Origin',(50.,40.8751692909919,4.53910246656033));
#10835=CARTESIAN_POINT('Origin',(36.,54.6122755947453,-11.9999999999999));
#10836=CARTESIAN_POINT('Origin',(36.,54.6122755947453,7.50000000000008));
#10837=CARTESIAN_POINT('Origin',(49.,54.6122755947453,-11.9999999999999));
#10838=CARTESIAN_POINT('Origin',(49.,54.6122755947453,7.50000000000009));
#10839=CARTESIAN_POINT('Origin',(34.999988,54.6122755947453,-11.9999999999999));
#10840=CARTESIAN_POINT('',(45.,54.6122755947453,5.50000000000009));
#10841=CARTESIAN_POINT('',(34.999988,54.6122755947453,5.50000000000008));
#10842=CARTESIAN_POINT('Origin',(45.,54.6122755947453,-11.9999999999999));
#10843=CARTESIAN_POINT('Origin',(45.,54.6122755947453,-11.9999999999999));
#10844=CARTESIAN_POINT('',(0.,0.,0.));
#10845=CARTESIAN_POINT('Origin',(50.,54.6122755947453,-11.9999999999999));
#10846=CARTESIAN_POINT('',(36.,54.6122755947453,-32.4999999999999));
#10847=CARTESIAN_POINT('',(36.,54.6122755947453,8.50000000000008));
#10848=CARTESIAN_POINT('Origin',(36.,54.6122755947453,-11.9999999999999));
#10849=CARTESIAN_POINT('Origin',(36.,54.6122755947453,-11.9999999999999));
#10850=CARTESIAN_POINT('',(36.603289189263,54.6122755947453,-32.4999999999999));
#10851=CARTESIAN_POINT('',(50.,54.6122755947453,-32.4999999999999));
#10852=CARTESIAN_POINT('',(36.7497490222913,54.2658144588871,-32.4970721002132));
#10853=CARTESIAN_POINT('Ctrl Pts',(36.7497490222914,54.2658144588871,-32.4970721002132));
#10854=CARTESIAN_POINT('Ctrl Pts',(36.7079677621958,54.3157388332819,-32.4979159697851));
#10855=CARTESIAN_POINT('Ctrl Pts',(36.6713203406449,54.3700115492414,-32.4986487617911));
#10856=CARTESIAN_POINT('Ctrl Pts',(36.6219970312668,54.4788517884076,-32.4996303938589));
#10857=CARTESIAN_POINT('Ctrl Pts',(36.6075439138862,54.5320464525539,-32.4999158675413));
#10858=CARTESIAN_POINT('Ctrl Pts',(36.6035546196614,54.5952824394035,-32.4999947523746));
#10859=CARTESIAN_POINT('Ctrl Pts',(36.6032891892631,54.6038064661215,-32.4999999999999));
#10860=CARTESIAN_POINT('Ctrl Pts',(36.6032891892631,54.6122755947453,-32.4999999999999));
#10861=CARTESIAN_POINT('',(48.396710810737,54.6122755947453,-32.4999999999999));
#10862=CARTESIAN_POINT('Ctrl Pts',(48.396710810737,54.6122755947453,-32.4999999999999));
#10863=CARTESIAN_POINT('Ctrl Pts',(48.396710810737,54.5998907719614,-32.4999999999999));
#10864=CARTESIAN_POINT('Ctrl Pts',(48.3961431217452,54.5874935361619,-32.4999887774468));
#10865=CARTESIAN_POINT('Ctrl Pts',(48.3891968128691,54.5117737928711,-32.4998514003519));
#10866=CARTESIAN_POINT('Ctrl Pts',(48.3690498018801,54.4529115279532,-32.4994531179785));
#10867=CARTESIAN_POINT('Ctrl Pts',(48.2945766533058,54.3105701888654,-32.49796779174));
#10868=CARTESIAN_POINT('Ctrl Pts',(48.224634010684,54.229506699135,-32.4965615873769));
#10869=CARTESIAN_POINT('Ctrl Pts',(47.9894682579553,54.0138621012104,-32.4917505532513));
#10870=CARTESIAN_POINT('Ctrl Pts',(47.790194476128,53.8921934273276,-32.4875698440548));
#10871=CARTESIAN_POINT('Ctrl Pts',(47.2591893370102,53.6095844257818,-32.4763245946928));
#10872=CARTESIAN_POINT('Ctrl Pts',(46.8036941106391,53.4296399345416,-32.4664417842137));
#10873=CARTESIAN_POINT('Ctrl Pts',(44.8908589619487,52.8583430003526,-32.4291083452159));
#10874=CARTESIAN_POINT('Ctrl Pts',(43.0234357271856,52.6236088262441,-32.4042961436254));
#10875=CARTESIAN_POINT('Ctrl Pts',(39.8390803845175,52.9459866017737,-32.4325402594283));
#10876=CARTESIAN_POINT('Ctrl Pts',(38.8321900018614,53.205505452804,-32.4535208321079));
#10877=CARTESIAN_POINT('Ctrl Pts',(37.7302514044692,53.6201478825653,-32.476460031332));
#10878=CARTESIAN_POINT('Ctrl Pts',(37.4193174431745,53.768280734008,-32.483158770581));
#10879=CARTESIAN_POINT('Ctrl Pts',(37.0379364071817,54.0043124559943,-32.4911694687953));
#10880=CARTESIAN_POINT('Ctrl Pts',(36.8894774405333,54.1120017210872,-32.4942401368472));
#10881=CARTESIAN_POINT('Ctrl Pts',(36.7699059821373,54.2423162108141,-32.4966645914004));
#10882=CARTESIAN_POINT('Ctrl Pts',(36.7596837012345,54.25394352369,-32.4968714463016));
#10883=CARTESIAN_POINT('Ctrl Pts',(36.7497490222914,54.2658144588871,-32.4970721002132));
#10884=CARTESIAN_POINT('',(49.,54.6122755947453,-32.4999999999999));
#10885=CARTESIAN_POINT('',(50.,54.6122755947453,-32.4999999999999));
#10886=CARTESIAN_POINT('',(49.,54.6122755947453,8.50000000000009));
#10887=CARTESIAN_POINT('Origin',(49.,54.6122755947453,-11.9999999999999));
#10888=CARTESIAN_POINT('Origin',(49.,54.6122755947453,-11.9999999999999));
#10889=CARTESIAN_POINT('Ctrl Pts',(36.603289189263,54.6122755947453,-32.4999999999999));
#10890=CARTESIAN_POINT('Ctrl Pts',(36.603289189263,54.6608249084485,-32.4999999999999));
#10891=CARTESIAN_POINT('Ctrl Pts',(36.6119924398781,54.7075701848921,-32.4998281802077));
#10892=CARTESIAN_POINT('Ctrl Pts',(36.6545156775753,54.8307810795885,-32.4989841905835));
#10893=CARTESIAN_POINT('Ctrl Pts',(36.7008380045797,54.9008048487387,-32.4980603157128));
#10894=CARTESIAN_POINT('Ctrl Pts',(36.8625317111402,55.0923640981108,-32.4947934283504));
#10895=CARTESIAN_POINT('Ctrl Pts',(37.0198338309866,55.2093236387767,-32.4915503477017));
#10896=CARTESIAN_POINT('Ctrl Pts',(37.4320685633155,55.4637121723344,-32.482889935361));
#10897=CARTESIAN_POINT('Ctrl Pts',(37.7488381293379,55.611880231403,-32.4760684685696));
#10898=CARTESIAN_POINT('Ctrl Pts',(39.1601676320809,56.1410407225304,-32.4467069002989));
#10899=CARTESIAN_POINT('Ctrl Pts',(40.717083195287,56.4741768433207,-32.4152718262714));
#10900=CARTESIAN_POINT('Ctrl Pts',(42.5,56.4741768433207,-32.4152718262714));
#10901=CARTESIAN_POINT('Ctrl Pts',(43.4574590376155,56.4741768433207,-32.4152718262714));
#10902=CARTESIAN_POINT('Ctrl Pts',(44.4269153217986,56.3794041517536,-32.4246324531227));
#10903=CARTESIAN_POINT('Ctrl Pts',(46.1871857836264,56.0096519365651,-32.4530673729712));
#10904=CARTESIAN_POINT('Ctrl Pts',(46.8757138664064,55.7779082090869,-32.4681777143441));
#10905=CARTESIAN_POINT('Ctrl Pts',(47.6009912659702,55.4395958991355,-32.4835638316369));
#10906=CARTESIAN_POINT('Ctrl Pts',(47.8399918525533,55.309998820274,-32.4886343233478));
#10907=CARTESIAN_POINT('Ctrl Pts',(48.1243771925797,55.091934993814,-32.4945190874943));
#10908=CARTESIAN_POINT('Ctrl Pts',(48.2195690308988,55.0050263124739,-32.4964575266732));
#10909=CARTESIAN_POINT('Ctrl Pts',(48.3274797628088,54.8557541081654,-32.4986259493983));
#10910=CARTESIAN_POINT('Ctrl Pts',(48.3595242538026,54.796889883988,-32.4992631372541));
#10911=CARTESIAN_POINT('Ctrl Pts',(48.3905089403897,54.6939813738137,-32.4998775530034));
#10912=CARTESIAN_POINT('Ctrl Pts',(48.396710810737,54.6531962409273,-32.4999999999999));
#10913=CARTESIAN_POINT('Ctrl Pts',(48.396710810737,54.6122755947453,-32.4999999999999));
#10914=CARTESIAN_POINT('',(36.5,41.5141044679107,3.76984188672031));
#10915=CARTESIAN_POINT('',(48.5,41.5141044679107,3.76984188672031));
#10916=CARTESIAN_POINT('',(48.5,41.5141044679107,3.76984188672031));
#10917=CARTESIAN_POINT('',(48.5,38.8424337080254,1.09817112683513));
#10918=CARTESIAN_POINT('Origin',(48.5,54.6122755947453,-11.9999999999999));
#10919=CARTESIAN_POINT('',(36.5,38.8424337080254,1.09817112683513));
#10920=CARTESIAN_POINT('',(48.5,38.8424337080254,1.09817112683513));
#10921=CARTESIAN_POINT('Origin',(36.5,54.6122755947453,-11.9999999999999));
#10922=CARTESIAN_POINT('',(36.5,38.8424337080252,-25.0981711268347));
#10923=CARTESIAN_POINT('',(48.5,38.8424337080252,-25.0981711268347));
#10924=CARTESIAN_POINT('',(48.5,38.8424337080252,-25.0981711268347));
#10925=CARTESIAN_POINT('',(48.5,41.5141044679105,-27.7698418867199));
#10926=CARTESIAN_POINT('Origin',(48.5,54.6122755947453,-11.9999999999999));
#10927=CARTESIAN_POINT('',(36.5,41.5141044679105,-27.7698418867199));
#10928=CARTESIAN_POINT('',(48.5,41.5141044679105,-27.7698418867199));
#10929=CARTESIAN_POINT('Origin',(36.5,54.6122755947453,-11.9999999999999));
#10930=CARTESIAN_POINT('',(36.5,67.7104467215801,-27.7698418867201));
#10931=CARTESIAN_POINT('',(48.5,67.7104467215801,-27.7698418867201));
#10932=CARTESIAN_POINT('',(48.5,67.7104467215801,-27.7698418867201));
#10933=CARTESIAN_POINT('',(48.5,70.3821174814653,-25.0981711268349));
#10934=CARTESIAN_POINT('Origin',(48.5,54.6122755947453,-11.9999999999999));
#10935=CARTESIAN_POINT('',(36.5,70.3821174814653,-25.0981711268349));
#10936=CARTESIAN_POINT('',(48.5,70.3821174814653,-25.0981711268349));
#10937=CARTESIAN_POINT('Origin',(36.5,54.6122755947453,-11.9999999999999));
#10938=CARTESIAN_POINT('',(36.5,70.3821174814654,1.09817112683487));
#10939=CARTESIAN_POINT('',(48.5,70.3821174814654,1.09817112683488));
#10940=CARTESIAN_POINT('',(48.5,70.3821174814654,1.09817112683488));
#10941=CARTESIAN_POINT('',(48.5,67.7104467215802,3.76984188672011));
#10942=CARTESIAN_POINT('Origin',(48.5,54.6122755947453,-11.9999999999999));
#10943=CARTESIAN_POINT('',(36.5,67.7104467215802,3.76984188672011));
#10944=CARTESIAN_POINT('',(48.5,67.7104467215802,3.76984188672011));
#10945=CARTESIAN_POINT('Origin',(36.5,54.6122755947453,-11.9999999999999));
#10946=CARTESIAN_POINT('',(36.7497652551312,75.1093469933142,-12.3464475251848));
#10947=CARTESIAN_POINT('Ctrl Pts',(42.5,75.0275474210168,-13.8619012485751));
#10948=CARTESIAN_POINT('Ctrl Pts',(41.5425409623847,75.0275474210168,-13.8619012485751));
#10949=CARTESIAN_POINT('Ctrl Pts',(40.5730846782014,75.0369080478681,-13.767128557008));
#10950=CARTESIAN_POINT('Ctrl Pts',(38.8128142163727,75.0653429677166,-13.3973763418193));
#10951=CARTESIAN_POINT('Ctrl Pts',(38.124286133593,75.0804533090896,-13.165632614341));
#10952=CARTESIAN_POINT('Ctrl Pts',(37.39900873403,75.0958394263824,-12.82732030439));
#10953=CARTESIAN_POINT('Ctrl Pts',(37.1600081474468,75.1009099180932,-12.6977232255284));
#10954=CARTESIAN_POINT('Ctrl Pts',(36.8756228074202,75.1067946822398,-12.4796593990683));
#10955=CARTESIAN_POINT('Ctrl Pts',(36.7804309691012,75.1087331214186,-12.3927507177283));
#10956=CARTESIAN_POINT('Ctrl Pts',(36.6725202371911,75.1109015441437,-12.2434785134197));
#10957=CARTESIAN_POINT('Ctrl Pts',(36.6404757461974,75.1115387319995,-12.1846142892423));
#10958=CARTESIAN_POINT('Ctrl Pts',(36.60578337376,75.1122266698925,-12.0693915532655));
#10959=CARTESIAN_POINT('Ctrl Pts',(36.6000950949635,75.1123387689502,-12.0162240743446));
#10960=CARTESIAN_POINT('Ctrl Pts',(36.6108031871309,75.1121269950974,-11.8994981981255));
#10961=CARTESIAN_POINT('Ctrl Pts',(36.63095019812,75.1117287127239,-11.8406359332075));
#10962=CARTESIAN_POINT('Ctrl Pts',(36.705423346694,75.1102433864854,-11.6982945941202));
#10963=CARTESIAN_POINT('Ctrl Pts',(36.7753659893155,75.1088371821223,-11.6172311043898));
#10964=CARTESIAN_POINT('Ctrl Pts',(37.0105317420447,75.1040261479967,-11.4015865064648));
#10965=CARTESIAN_POINT('Ctrl Pts',(37.2098055238719,75.0998454388001,-11.279917832582));
#10966=CARTESIAN_POINT('Ctrl Pts',(37.7408106629901,75.0886001894382,-10.997308831036));
#10967=CARTESIAN_POINT('Ctrl Pts',(38.1963058893614,75.0787173789591,-10.8173643397959));
#10968=CARTESIAN_POINT('Ctrl Pts',(40.1091410380511,75.0413839399612,-10.2460674056071));
#10969=CARTESIAN_POINT('Ctrl Pts',(41.9765642728142,75.0165717383708,-10.0113332314985));
#10970=CARTESIAN_POINT('Ctrl Pts',(45.1609196154824,75.0448158541737,-10.3337110070281));
#10971=CARTESIAN_POINT('Ctrl Pts',(46.1678099981386,75.0657964268533,-10.5932298580583));
#10972=CARTESIAN_POINT('Ctrl Pts',(47.2697485955313,75.0887356260774,-11.0078722878199));
#10973=CARTESIAN_POINT('Ctrl Pts',(47.5806825568259,75.0954343653265,-11.1560051392625));
#10974=CARTESIAN_POINT('Ctrl Pts',(47.9620635928186,75.1034450635407,-11.3920368612488));
#10975=CARTESIAN_POINT('Ctrl Pts',(48.1105225594667,75.1065157315926,-11.4997261263416));
#10976=CARTESIAN_POINT('Ctrl Pts',(48.2739688645561,75.10982980122,-11.6778574474043));
#10977=CARTESIAN_POINT('Ctrl Pts',(48.3224965288387,75.1108012999275,-11.7440918293815));
#10978=CARTESIAN_POINT('Ctrl Pts',(48.3780029687331,75.1119059886043,-11.8665761936618));
#10979=CARTESIAN_POINT('Ctrl Pts',(48.3924560861139,75.1121914622867,-11.9197708578082));
#10980=CARTESIAN_POINT('Ctrl Pts',(48.3995482155258,75.1123317029947,-12.0321911950802));
#10981=CARTESIAN_POINT('Ctrl Pts',(48.3907243897671,75.112157697847,-12.0874225881673));
#10982=CARTESIAN_POINT('Ctrl Pts',(48.3454843224248,75.111259785329,-12.2185054848428));
#10983=CARTESIAN_POINT('Ctrl Pts',(48.2991619954204,75.1103359104582,-12.2885292539931));
#10984=CARTESIAN_POINT('Ctrl Pts',(48.1374682888594,75.1070690230958,-12.4800885033658));
#10985=CARTESIAN_POINT('Ctrl Pts',(47.9801661690123,75.1038259424471,-12.5970480440319));
#10986=CARTESIAN_POINT('Ctrl Pts',(47.567931436684,75.0951655301064,-12.8514365775891));
#10987=CARTESIAN_POINT('Ctrl Pts',(47.2511618706613,75.088344063315,-12.9996046366577));
#10988=CARTESIAN_POINT('Ctrl Pts',(45.8398323679192,75.0589824950443,-13.5287651277848));
#10989=CARTESIAN_POINT('Ctrl Pts',(44.2829168047132,75.0275474210168,-13.8619012485751));
#10990=CARTESIAN_POINT('Ctrl Pts',(42.5,75.0275474210168,-13.8619012485751));
#10991=CARTESIAN_POINT('',(36.7497162970046,54.2657870626157,8.49707235020499));
#10992=CARTESIAN_POINT('Ctrl Pts',(42.5,56.4741768433204,8.41527182627157));
#10993=CARTESIAN_POINT('Ctrl Pts',(41.5425409623847,56.4741768433204,8.41527182627157));
#10994=CARTESIAN_POINT('Ctrl Pts',(40.5730846782016,56.3794041517534,8.42463245312286));
#10995=CARTESIAN_POINT('Ctrl Pts',(38.8128142163725,56.0096519365646,8.45306737297136));
#10996=CARTESIAN_POINT('Ctrl Pts',(38.1242861335929,55.7779082090862,8.46817771434433));
#10997=CARTESIAN_POINT('Ctrl Pts',(37.3990087340298,55.4395958991352,8.48356383163711));
#10998=CARTESIAN_POINT('Ctrl Pts',(37.1600081474467,55.3099988202737,8.48863432334797));
#10999=CARTESIAN_POINT('Ctrl Pts',(36.8756228074202,55.0919349938136,8.49451908749452));
#11000=CARTESIAN_POINT('Ctrl Pts',(36.7804309691012,55.0050263124736,8.49645752667339));
#11001=CARTESIAN_POINT('Ctrl Pts',(36.6725202371913,54.8557541081652,8.49862594939842));
#11002=CARTESIAN_POINT('Ctrl Pts',(36.6404757461974,54.7968898839877,8.49926313725424));
#11003=CARTESIAN_POINT('Ctrl Pts',(36.60578337376,54.6816671480108,8.4999510751473));
#11004=CARTESIAN_POINT('Ctrl Pts',(36.6000950949635,54.6284996690899,8.50006317420492));
#11005=CARTESIAN_POINT('Ctrl Pts',(36.6108031871309,54.5117737928708,8.4998514003521));
#11006=CARTESIAN_POINT('Ctrl Pts',(36.63095019812,54.4529115279528,8.49945311797868));
#11007=CARTESIAN_POINT('Ctrl Pts',(36.7054233466942,54.3105701888652,8.49796779174013));
#11008=CARTESIAN_POINT('Ctrl Pts',(36.7753659893159,54.2295066991348,8.49656158737708));
#11009=CARTESIAN_POINT('Ctrl Pts',(37.0105317420448,54.01386210121,8.49175055325143));
#11010=CARTESIAN_POINT('Ctrl Pts',(37.2098055238722,53.8921934273273,8.48756984405489));
#11011=CARTESIAN_POINT('Ctrl Pts',(37.7408106629893,53.6095844257818,8.47632459469298));
#11012=CARTESIAN_POINT('Ctrl Pts',(38.1963058893602,53.4296399345416,8.46644178421388));
#11013=CARTESIAN_POINT('Ctrl Pts',(40.1091410380517,52.8583430003522,8.42910834521598));
#11014=CARTESIAN_POINT('Ctrl Pts',(41.9765642728151,52.623608826244,8.40429614362558));
#11015=CARTESIAN_POINT('Ctrl Pts',(45.1609196154835,52.9459866017735,8.43254025942847));
#11016=CARTESIAN_POINT('Ctrl Pts',(46.1678099981393,53.2055054528039,8.45352083210801));
#11017=CARTESIAN_POINT('Ctrl Pts',(47.2697485955285,53.6201478825642,8.47646003133207));
#11018=CARTESIAN_POINT('Ctrl Pts',(47.5806825568242,53.7682807340069,8.48315877058117));
#11019=CARTESIAN_POINT('Ctrl Pts',(47.9620635928186,54.0043124559941,8.49116946879544));
#11020=CARTESIAN_POINT('Ctrl Pts',(48.1105225594668,54.112001721087,8.49424013684733));
#11021=CARTESIAN_POINT('Ctrl Pts',(48.2739688645561,54.2901330421496,8.49755420647477));
#11022=CARTESIAN_POINT('Ctrl Pts',(48.3224965288387,54.3563674241268,8.49852570518227));
#11023=CARTESIAN_POINT('Ctrl Pts',(48.3780029687332,54.4788517884074,8.49963039385909));
#11024=CARTESIAN_POINT('Ctrl Pts',(48.3924560861139,54.5320464525537,8.49991586754141));
#11025=CARTESIAN_POINT('Ctrl Pts',(48.3995482155258,54.6444667898256,8.50005610824948));
#11026=CARTESIAN_POINT('Ctrl Pts',(48.390724389767,54.6996981829127,8.49988210310169));
#11027=CARTESIAN_POINT('Ctrl Pts',(48.3454843224248,54.8307810795882,8.49898419058371));
#11028=CARTESIAN_POINT('Ctrl Pts',(48.2991619954204,54.9008048487383,8.498060315713));
#11029=CARTESIAN_POINT('Ctrl Pts',(48.13746828886,55.0923640981104,8.49479342835062));
#11030=CARTESIAN_POINT('Ctrl Pts',(47.9801661690137,55.2093236387763,8.49155034770193));
#11031=CARTESIAN_POINT('Ctrl Pts',(47.5679314366844,55.4637121723342,8.48288993536117));
#11032=CARTESIAN_POINT('Ctrl Pts',(47.251161870662,55.6118802314028,8.47606846856981));
#11033=CARTESIAN_POINT('Ctrl Pts',(45.8398323679184,56.1410407225304,8.4467069002991));
#11034=CARTESIAN_POINT('Ctrl Pts',(44.2829168047119,56.4741768433204,8.41527182627157));
#11035=CARTESIAN_POINT('Ctrl Pts',(42.5,56.4741768433204,8.41527182627157));
#11036=CARTESIAN_POINT('',(36.7497162970046,34.1152032445404,-12.3464885321295));
#11037=CARTESIAN_POINT('Ctrl Pts',(42.5,34.1970037684738,-10.1380987514247));
#11038=CARTESIAN_POINT('Ctrl Pts',(41.5425409623847,34.1970037684738,-10.1380987514247));
#11039=CARTESIAN_POINT('Ctrl Pts',(40.5730846782015,34.1876431416225,-10.2328714429918));
#11040=CARTESIAN_POINT('Ctrl Pts',(38.8128142163735,34.1592082217741,-10.6026236581803));
#11041=CARTESIAN_POINT('Ctrl Pts',(38.1242861335935,34.1440978804011,-10.8343673856586));
#11042=CARTESIAN_POINT('Ctrl Pts',(37.39900873403,34.1287117631083,-11.1726796956099));
#11043=CARTESIAN_POINT('Ctrl Pts',(37.1600081474469,34.1236412713974,-11.3022767744714));
#11044=CARTESIAN_POINT('Ctrl Pts',(36.8756228074203,34.1177565072509,-11.5203406009315));
#11045=CARTESIAN_POINT('Ctrl Pts',(36.7804309691013,34.115818068072,-11.6072492822715));
#11046=CARTESIAN_POINT('Ctrl Pts',(36.6725202371913,34.113649645347,-11.75652148658));
#11047=CARTESIAN_POINT('Ctrl Pts',(36.6404757461974,34.1130124574912,-11.8153857107575));
#11048=CARTESIAN_POINT('Ctrl Pts',(36.60578337376,34.1123245195981,-11.9306084467343));
#11049=CARTESIAN_POINT('Ctrl Pts',(36.6000950949635,34.1122124205405,-11.9837759256552));
#11050=CARTESIAN_POINT('Ctrl Pts',(36.6108031871309,34.1124241943933,-12.1005018018743));
#11051=CARTESIAN_POINT('Ctrl Pts',(36.63095019812,34.1128224767667,-12.1593640667924));
#11052=CARTESIAN_POINT('Ctrl Pts',(36.7054233466949,34.1143078030053,-12.3017054058813));
#11053=CARTESIAN_POINT('Ctrl Pts',(36.7753659893176,34.1157140073684,-12.3827688956119));
#11054=CARTESIAN_POINT('Ctrl Pts',(37.0105317420447,34.120525041494,-12.598413493535));
#11055=CARTESIAN_POINT('Ctrl Pts',(37.2098055238719,34.1247057506905,-12.7200821674178));
#11056=CARTESIAN_POINT('Ctrl Pts',(37.7408106629894,34.1359510000524,-13.0026911689634));
#11057=CARTESIAN_POINT('Ctrl Pts',(38.1963058893603,34.1458338105315,-13.1826356602036));
#11058=CARTESIAN_POINT('Ctrl Pts',(40.1091410380501,34.1831672495294,-13.7539325943925));
#11059=CARTESIAN_POINT('Ctrl Pts',(41.9765642728128,34.2079794511198,-13.9886667685015));
#11060=CARTESIAN_POINT('Ctrl Pts',(45.160919615482,34.1797353353169,-13.6662889929718));
#11061=CARTESIAN_POINT('Ctrl Pts',(46.1678099981384,34.1587547626374,-13.4067701419416));
#11062=CARTESIAN_POINT('Ctrl Pts',(47.2697485955313,34.1358155634133,-12.99212771218));
#11063=CARTESIAN_POINT('Ctrl Pts',(47.5806825568258,34.1291168241642,-12.8439948607373));
#11064=CARTESIAN_POINT('Ctrl Pts',(47.9620635928185,34.12110612595,-12.6079631387512));
#11065=CARTESIAN_POINT('Ctrl Pts',(48.1105225594667,34.1180354578981,-12.5002738736583));
#11066=CARTESIAN_POINT('Ctrl Pts',(48.273968864556,34.1147213882706,-12.3221425525957));
#11067=CARTESIAN_POINT('Ctrl Pts',(48.3224965288387,34.1137498895631,-12.2559081706184));
#11068=CARTESIAN_POINT('Ctrl Pts',(48.3780029687333,34.1126452008863,-12.1334238063378));
#11069=CARTESIAN_POINT('Ctrl Pts',(48.3924560861139,34.112359727204,-12.0802291421916));
#11070=CARTESIAN_POINT('Ctrl Pts',(48.3995482155258,34.1122194864959,-11.9678088049197));
#11071=CARTESIAN_POINT('Ctrl Pts',(48.3907243897671,34.1123934916437,-11.9125774118326));
#11072=CARTESIAN_POINT('Ctrl Pts',(48.3454843224248,34.1132914041617,-11.7814945151571));
#11073=CARTESIAN_POINT('Ctrl Pts',(48.2991619954205,34.1142152790324,-11.7114707460069));
#11074=CARTESIAN_POINT('Ctrl Pts',(48.1374682888603,34.1174821663948,-11.5199114966352));
#11075=CARTESIAN_POINT('Ctrl Pts',(47.9801661690144,34.1207252470435,-11.4029519559693));
#11076=CARTESIAN_POINT('Ctrl Pts',(47.5679314366847,34.1293856593842,-11.1485634224112));
#11077=CARTESIAN_POINT('Ctrl Pts',(47.2511618706624,34.1362071261756,-11.0003953633426));
#11078=CARTESIAN_POINT('Ctrl Pts',(45.8398323679199,34.1655686944463,-10.4712348722153));
#11079=CARTESIAN_POINT('Ctrl Pts',(44.2829168047143,34.1970037684738,-10.1380987514247));
#11080=CARTESIAN_POINT('Ctrl Pts',(42.5,34.1970037684738,-10.1380987514247));
#11081=CARTESIAN_POINT('Origin',(50.,54.6122755947453,-11.9999999999999));
#11082=CARTESIAN_POINT('',(50.,54.6122755947453,7.50000000000009));
#11083=CARTESIAN_POINT('Origin',(50.,54.6122755947453,-11.9999999999999));
#11084=CARTESIAN_POINT('',(50.,54.6122755947453,5.50000000000008));
#11085=CARTESIAN_POINT('Origin',(50.,54.6122755947453,-11.9999999999999));
#11086=CARTESIAN_POINT('Origin',(35.,54.6122755947453,-11.9999999999999));
#11087=CARTESIAN_POINT('',(35.,54.6122755947453,7.50000000000008));
#11088=CARTESIAN_POINT('Origin',(35.,54.6122755947453,-11.9999999999999));
#11089=CARTESIAN_POINT('',(35.,54.6122755947453,5.50000000000008));
#11090=CARTESIAN_POINT('Origin',(35.,54.6122755947453,-11.9999999999999));
#11091=CARTESIAN_POINT('Ctrl Pts',(36.6000954047721,75.6303323723191,-11.0710623055408));
#11092=CARTESIAN_POINT('Ctrl Pts',(36.6000954047721,75.1163129851934,-11.390036451076));
#11093=CARTESIAN_POINT('Ctrl Pts',(36.6000954047721,75.113533389205,-11.9949767040821));
#11094=CARTESIAN_POINT('Ctrl Pts',(36.6000954047721,75.1107537932165,-12.5999169570882));
#11095=CARTESIAN_POINT('Ctrl Pts',(36.6000954047721,75.6218202760576,-12.923601195162));
#11096=CARTESIAN_POINT('Ctrl Pts',(42.4997945641984,74.4160919611753,-9.11434223685902));
#11097=CARTESIAN_POINT('Ctrl Pts',(42.4997945641984,72.8193389779435,-10.1052054829035));
#11098=CARTESIAN_POINT('Ctrl Pts',(42.4997945641984,72.8107044238821,-11.9843956026886));
#11099=CARTESIAN_POINT('Ctrl Pts',(42.4997945641984,72.8020698698207,-13.8635857224736));
#11100=CARTESIAN_POINT('Ctrl Pts',(42.4997945641984,74.3896499330349,-14.8690804289273));
#11101=CARTESIAN_POINT('Ctrl Pts',(48.3995480441881,75.630258991695,-11.0709440543786));
#11102=CARTESIAN_POINT('Ctrl Pts',(48.3995480441881,75.1161741713435,-11.3899588044276));
#11103=CARTESIAN_POINT('Ctrl Pts',(48.3995480441881,75.1133942215203,-11.9949760646306));
#11104=CARTESIAN_POINT('Ctrl Pts',(48.3995480441881,75.1106142716971,-12.5999933248336));
#11105=CARTESIAN_POINT('Ctrl Pts',(48.3995480441881,75.6217458118676,-12.9237187670028));
#11106=CARTESIAN_POINT('Ctrl Pts',(36.6000954047721,53.6833379002862,9.01805677757378));
#11107=CARTESIAN_POINT('Ctrl Pts',(36.6000954047721,54.0023120458214,8.50403739044816));
#11108=CARTESIAN_POINT('Ctrl Pts',(36.6000954047721,54.6072522988275,8.50125779445973));
#11109=CARTESIAN_POINT('Ctrl Pts',(36.6000954047721,55.2121925518336,8.4984781984713));
#11110=CARTESIAN_POINT('Ctrl Pts',(36.6000954047721,55.5358767899073,9.00954468131236));
#11111=CARTESIAN_POINT('Ctrl Pts',(42.4997945641984,51.7266178316045,7.80381636642986));
#11112=CARTESIAN_POINT('Ctrl Pts',(42.4997945641984,52.7174810776491,6.2070633831982));
#11113=CARTESIAN_POINT('Ctrl Pts',(42.4997945641984,54.596671197434,6.19842882913689));
#11114=CARTESIAN_POINT('Ctrl Pts',(42.4997945641984,56.4758613172189,6.18979427507558));
#11115=CARTESIAN_POINT('Ctrl Pts',(42.4997945641984,57.4813560236726,7.77737433828968));
#11116=CARTESIAN_POINT('Ctrl Pts',(48.3995480441881,53.683219649124,9.0179833969497));
#11117=CARTESIAN_POINT('Ctrl Pts',(48.3995480441881,54.002234399173,8.50389857659829));
#11118=CARTESIAN_POINT('Ctrl Pts',(48.3995480441881,54.607251659376,8.50111862677509));
#11119=CARTESIAN_POINT('Ctrl Pts',(48.3995480441881,55.212268919579,8.49833867695189));
#11120=CARTESIAN_POINT('Ctrl Pts',(48.3995480441881,55.5359943617481,9.00947021712231));
#11121=CARTESIAN_POINT('Ctrl Pts',(36.6000954047722,33.5942188171715,-12.9289376944591));
#11122=CARTESIAN_POINT('Ctrl Pts',(36.6000954047722,34.1082382042972,-12.6099635489239));
#11123=CARTESIAN_POINT('Ctrl Pts',(36.6000954047722,34.1110178002857,-12.0050232959178));
#11124=CARTESIAN_POINT('Ctrl Pts',(36.6000954047722,34.1137973962741,-11.4000830429116));
#11125=CARTESIAN_POINT('Ctrl Pts',(36.6000954047722,33.602730913433,-11.0763988048379));
#11126=CARTESIAN_POINT('Ctrl Pts',(42.4997945641985,34.8084592283153,-14.8856577631409));
#11127=CARTESIAN_POINT('Ctrl Pts',(42.4997945641985,36.4052122115471,-13.8947945170964));
#11128=CARTESIAN_POINT('Ctrl Pts',(42.4997945641985,36.4138467656085,-12.0156043973113));
#11129=CARTESIAN_POINT('Ctrl Pts',(42.4997945641985,36.4224813196699,-10.1364142775263));
#11130=CARTESIAN_POINT('Ctrl Pts',(42.4997945641985,34.8349012564557,-9.13091957107256));
#11131=CARTESIAN_POINT('Ctrl Pts',(48.3995480441881,33.5942921977956,-12.9290559456212));
#11132=CARTESIAN_POINT('Ctrl Pts',(48.3995480441881,34.1083770181471,-12.6100411955723));
#11133=CARTESIAN_POINT('Ctrl Pts',(48.3995480441881,34.1111569679703,-12.0050239353692));
#11134=CARTESIAN_POINT('Ctrl Pts',(48.3995480441881,34.1139369177935,-11.4000066751662));
#11135=CARTESIAN_POINT('Ctrl Pts',(48.3995480441881,33.6028053776231,-11.0762812329971));
#11136=CARTESIAN_POINT('Ctrl Pts',(36.603289189263,55.5369296408085,-33.0088778576148));
#11137=CARTESIAN_POINT('Ctrl Pts',(36.603289189263,55.2128764217899,-32.4972287891192));
#11138=CARTESIAN_POINT('Ctrl Pts',(36.603289189263,54.6072465725666,-32.5000115536831));
#11139=CARTESIAN_POINT('Ctrl Pts',(36.603289189263,54.0016167233433,-32.5027943182471));
#11140=CARTESIAN_POINT('Ctrl Pts',(36.603289189263,53.682278966091,-33.0173996571641));
#11141=CARTESIAN_POINT('Ctrl Pts',(42.5,57.4802106040728,-31.7780997904234));
#11142=CARTESIAN_POINT('Ctrl Pts',(42.5,56.4751173200863,-30.1911535349279));
#11143=CARTESIAN_POINT('Ctrl Pts',(42.5,54.5966774271594,-30.1997846418264));
#11144=CARTESIAN_POINT('Ctrl Pts',(42.5,52.7182375342324,-30.2084157487249));
#11145=CARTESIAN_POINT('Ctrl Pts',(42.5,51.7277698693544,-31.8045312621439));
#11146=CARTESIAN_POINT('Ctrl Pts',(48.396710810737,55.5369296408085,-33.0088778576148));
#11147=CARTESIAN_POINT('Ctrl Pts',(48.396710810737,55.2128764217899,-32.4972287891192));
#11148=CARTESIAN_POINT('Ctrl Pts',(48.396710810737,54.6072465725666,-32.5000115536831));
#11149=CARTESIAN_POINT('Ctrl Pts',(48.396710810737,54.0016167233433,-32.5027943182471));
#11150=CARTESIAN_POINT('Ctrl Pts',(48.396710810737,53.682278966091,-33.0173996571641));
#11151=CARTESIAN_POINT('Origin',(47.5,69.4571012113211,2.84482561657582));
#11152=CARTESIAN_POINT('',(47.5,70.4387355541152,2.55242815321436));
#11153=CARTESIAN_POINT('',(47.5,69.1647037479597,3.82645995936986));
#11154=CARTESIAN_POINT('Origin',(47.5,69.4571012113211,2.84482561657582));
#11155=CARTESIAN_POINT('',(47.537899429919,70.3143910047143,2.28432898886365));
#11156=CARTESIAN_POINT('Ctrl Pts',(47.5,70.4387355541152,2.55242815321436));
#11157=CARTESIAN_POINT('Ctrl Pts',(47.5,70.4189527998948,2.48601365455714));
#11158=CARTESIAN_POINT('Ctrl Pts',(47.5053044417601,70.3925771182096,2.422112506851));
#11159=CARTESIAN_POINT('Ctrl Pts',(47.5230476022983,70.3458637388305,2.33479395638985));
#11160=CARTESIAN_POINT('Ctrl Pts',(47.5298073931343,70.3305302530218,2.30901426289197));
#11161=CARTESIAN_POINT('Ctrl Pts',(47.537899429919,70.3143910047143,2.28432898886365));
#11162=CARTESIAN_POINT('',(37.4621005700809,70.3143910047143,2.28432898886365));
#11163=CARTESIAN_POINT('',(47.537899429919,70.3143910047143,2.28432898886365));
#11164=CARTESIAN_POINT('',(37.5,70.4387355541152,2.55242815321436));
#11165=CARTESIAN_POINT('Ctrl Pts',(37.462100570081,70.3143910047143,2.28432898886366));
#11166=CARTESIAN_POINT('Ctrl Pts',(37.4632744099609,70.3167321820717,2.28790986224227));
#11167=CARTESIAN_POINT('Ctrl Pts',(37.4644207388779,70.3190574281895,2.29151535342116));
#11168=CARTESIAN_POINT('Ctrl Pts',(37.4898409184866,70.371513910436,2.37399296978792));
#11169=CARTESIAN_POINT('Ctrl Pts',(37.5,70.4113518729136,2.46049588543571));
#11170=CARTESIAN_POINT('Ctrl Pts',(37.5,70.4387355541152,2.55242815321435));
#11171=CARTESIAN_POINT('',(37.5,69.1647037479597,3.82645995936986));
#11172=CARTESIAN_POINT('Origin',(37.5,69.4571012113211,2.84482561657581));
#11173=CARTESIAN_POINT('',(37.4621005700809,68.8966045836089,3.70211540996904));
#11174=CARTESIAN_POINT('Ctrl Pts',(37.5,69.1647037479597,3.82645995936986));
#11175=CARTESIAN_POINT('Ctrl Pts',(37.5,69.0990912208333,3.80691608680946));
#11176=CARTESIAN_POINT('Ctrl Pts',(37.4948229521317,69.0359160073849,3.78093293985881));
#11177=CARTESIAN_POINT('Ctrl Pts',(37.4773121076774,68.948446705185,3.73440602894735));
#11178=CARTESIAN_POINT('Ctrl Pts',(37.470409170669,68.9219504993238,3.7186865862433));
#11179=CARTESIAN_POINT('Ctrl Pts',(37.462100570081,68.896604583609,3.70211540996904));
#11180=CARTESIAN_POINT('',(47.5378994299191,68.8966045836089,3.70211540996904));
#11181=CARTESIAN_POINT('',(47.5378994299191,68.8966045836089,3.70211540996904));
#11182=CARTESIAN_POINT('Ctrl Pts',(47.537899429919,68.8966045836089,3.70211540996903));
#11183=CARTESIAN_POINT('Ctrl Pts',(47.5369318666484,68.8995561970421,3.7040451767624));
#11184=CARTESIAN_POINT('Ctrl Pts',(47.5359829808858,68.9025245795757,3.7059641473824));
#11185=CARTESIAN_POINT('Ctrl Pts',(47.510332174293,68.9848409778267,3.75857431922063));
#11186=CARTESIAN_POINT('Ctrl Pts',(47.5,69.0719944289914,3.79884481948067));
#11187=CARTESIAN_POINT('Ctrl Pts',(47.5,69.1647037479597,3.82645995936986));
#11188=CARTESIAN_POINT('Origin',(47.5,54.6122755947453,-11.9999999999999));
#11189=CARTESIAN_POINT('Origin',(47.5,54.6122755947453,-11.9999999999999));
#11190=CARTESIAN_POINT('Origin',(37.5,54.6122755947453,-11.9999999999999));
#11191=CARTESIAN_POINT('Origin',(37.5,54.6122755947453,-11.9999999999999));
#11192=CARTESIAN_POINT('Origin',(47.5,68.349381898499,4.5391024665601));
#11193=CARTESIAN_POINT('Ctrl Pts',(37.4621005700809,68.896604583609,3.70211540996902));
#11194=CARTESIAN_POINT('Ctrl Pts',(37.4310083838403,68.8017558875511,3.6401032704416));
#11195=CARTESIAN_POINT('Ctrl Pts',(37.3828779782886,68.7018867262922,3.59772631179564));
#11196=CARTESIAN_POINT('Ctrl Pts',(37.245031822289,68.4694900791145,3.53679150015867));
#11197=CARTESIAN_POINT('Ctrl Pts',(37.1423703640038,68.3305669520952,3.52988534954539));
#11198=CARTESIAN_POINT('Ctrl Pts',(36.8667626334574,68.017493954875,3.57885731564907));
#11199=CARTESIAN_POINT('Ctrl Pts',(36.6872103879512,67.8515747651484,3.65364745765698));
#11200=CARTESIAN_POINT('Ctrl Pts',(36.5029780432796,67.7126857281249,3.76798632698662));
#11201=CARTESIAN_POINT('Ctrl Pts',(36.5014890205786,67.711565210995,3.76891288782061));
#11202=CARTESIAN_POINT('Ctrl Pts',(36.5,67.7104467215802,3.76984188672011));
#11203=CARTESIAN_POINT('Ctrl Pts',(47.537899429919,68.896604583609,3.70211540996901));
#11204=CARTESIAN_POINT('Ctrl Pts',(47.5689916161593,68.8017558875522,3.64010327044235));
#11205=CARTESIAN_POINT('Ctrl Pts',(47.6171220217102,68.7018867262946,3.59772631179665));
#11206=CARTESIAN_POINT('Ctrl Pts',(47.7549681777082,68.4694900791187,3.53679150015924));
#11207=CARTESIAN_POINT('Ctrl Pts',(47.8576296359926,68.3305669520998,3.52988534954533));
#11208=CARTESIAN_POINT('Ctrl Pts',(48.1332373665856,68.0174939548254,3.57885731565596));
#11209=CARTESIAN_POINT('Ctrl Pts',(48.3127896121225,67.8515747651177,3.65364745768193));
#11210=CARTESIAN_POINT('Ctrl Pts',(48.4970219567203,67.7126857281242,3.76798632698724));
#11211=CARTESIAN_POINT('Ctrl Pts',(48.498510979422,67.7115652109945,3.76891288782097));
#11212=CARTESIAN_POINT('Ctrl Pts',(48.5,67.7104467215802,3.7698418867201));
#11213=CARTESIAN_POINT('Origin',(48.5,54.6122755947453,-11.9999999999999));
#11214=CARTESIAN_POINT('Ctrl Pts',(47.537899429919,70.3143910047143,2.28432898886365));
#11215=CARTESIAN_POINT('Ctrl Pts',(47.5689916161588,70.2523788651886,2.18948029280836));
#11216=CARTESIAN_POINT('Ctrl Pts',(47.6171220217088,70.2100019065432,2.08961113155225));
#11217=CARTESIAN_POINT('Ctrl Pts',(47.7549681777051,70.1490670949051,1.85721448437786));
#11218=CARTESIAN_POINT('Ctrl Pts',(47.8576296359887,70.1421609442907,1.71829135735951));
#11219=CARTESIAN_POINT('Ctrl Pts',(48.1332373666213,70.1911329104067,1.40521836003877));
#11220=CARTESIAN_POINT('Ctrl Pts',(48.3127896121854,70.2659230524474,1.23929917034817));
#11221=CARTESIAN_POINT('Ctrl Pts',(48.4970219567186,70.3802619217321,1.10041013337938));
#11222=CARTESIAN_POINT('Ctrl Pts',(48.4985109794219,70.3811884825662,1.09928961624927));
#11223=CARTESIAN_POINT('Ctrl Pts',(48.5,70.3821174814654,1.09817112683487));
#11224=CARTESIAN_POINT('Origin',(36.5,54.6122755947453,-11.9999999999999));
#11225=CARTESIAN_POINT('Ctrl Pts',(37.4621005700809,70.3143910047143,2.28432898886365));
#11226=CARTESIAN_POINT('Ctrl Pts',(37.4310083838412,70.2523788651887,2.18948029280845));
#11227=CARTESIAN_POINT('Ctrl Pts',(37.3828779782913,70.2100019065433,2.08961113155242));
#11228=CARTESIAN_POINT('Ctrl Pts',(37.2450318222954,70.1490670949052,1.85721448437858));
#11229=CARTESIAN_POINT('Ctrl Pts',(37.1423703640119,70.1421609442906,1.71829135736027));
#11230=CARTESIAN_POINT('Ctrl Pts',(36.8667626333773,70.1911329104068,1.40521836003708));
#11231=CARTESIAN_POINT('Ctrl Pts',(36.6872103878129,70.2659230524489,1.23929917034637));
#11232=CARTESIAN_POINT('Ctrl Pts',(36.5029780432807,70.3802619217326,1.10041013337885));
#11233=CARTESIAN_POINT('Ctrl Pts',(36.5014890205792,70.3811884825656,1.09928961625003));
#11234=CARTESIAN_POINT('Ctrl Pts',(36.5,70.3821174814654,1.09817112683487));
#11235=CARTESIAN_POINT('Origin',(50.,71.1513780613054,1.73710630375365));
#11236=CARTESIAN_POINT('Origin',(47.5,39.7674499781698,2.84482561657604));
#11237=CARTESIAN_POINT('',(47.5,40.0598474415312,3.82645995937007));
#11238=CARTESIAN_POINT('',(47.5,38.7858156353757,2.5524281532146));
#11239=CARTESIAN_POINT('Origin',(47.5,39.7674499781698,2.84482561657604));
#11240=CARTESIAN_POINT('',(47.5378994299191,40.3279466058819,3.70211540996925));
#11241=CARTESIAN_POINT('Ctrl Pts',(47.5,40.0598474415312,3.82645995937007));
#11242=CARTESIAN_POINT('Ctrl Pts',(47.5,40.1262619401886,3.80667720514962));
#11243=CARTESIAN_POINT('Ctrl Pts',(47.5053044417602,40.1901630878949,3.7803015234644));
#11244=CARTESIAN_POINT('Ctrl Pts',(47.5230476022984,40.277481638356,3.73358814408523));
#11245=CARTESIAN_POINT('Ctrl Pts',(47.5298073931343,40.3032613318537,3.71825465827663));
#11246=CARTESIAN_POINT('Ctrl Pts',(47.537899429919,40.3279466058819,3.70211540996925));
#11247=CARTESIAN_POINT('',(37.462100570081,40.3279466058819,3.70211540996925));
#11248=CARTESIAN_POINT('',(47.5378994299191,40.3279466058819,3.70211540996925));
#11249=CARTESIAN_POINT('',(37.5,40.0598474415312,3.82645995937007));
#11250=CARTESIAN_POINT('Ctrl Pts',(37.462100570081,40.3279466058819,3.70211540996925));
#11251=CARTESIAN_POINT('Ctrl Pts',(37.4632744099609,40.3243657325033,3.70445658732663));
#11252=CARTESIAN_POINT('Ctrl Pts',(37.4644207388779,40.3207602413243,3.70678183344449));
#11253=CARTESIAN_POINT('Ctrl Pts',(37.4898409184866,40.2382826249574,3.75923831569102));
#11254=CARTESIAN_POINT('Ctrl Pts',(37.5,40.1517797093097,3.7990762781686));
#11255=CARTESIAN_POINT('Ctrl Pts',(37.5,40.0598474415312,3.82645995937007));
#11256=CARTESIAN_POINT('',(37.5,38.7858156353757,2.55242815321459));
#11257=CARTESIAN_POINT('Origin',(37.5,39.7674499781698,2.84482561657603));
#11258=CARTESIAN_POINT('',(37.462100570081,38.9101601847765,2.28432898886388));
#11259=CARTESIAN_POINT('Ctrl Pts',(37.5,38.7858156353757,2.55242815321459));
#11260=CARTESIAN_POINT('Ctrl Pts',(37.5,38.8053595079361,2.48681562608814));
#11261=CARTESIAN_POINT('Ctrl Pts',(37.4948229521316,38.8313426548868,2.42364041263967));
#11262=CARTESIAN_POINT('Ctrl Pts',(37.4773121076774,38.8778695657982,2.33617111043986));
#11263=CARTESIAN_POINT('Ctrl Pts',(37.470409170669,38.8935890085023,2.3096749045787));
#11264=CARTESIAN_POINT('Ctrl Pts',(37.462100570081,38.9101601847765,2.28432898886388));
#11265=CARTESIAN_POINT('',(47.5378994299191,38.9101601847765,2.28432898886388));
#11266=CARTESIAN_POINT('',(47.5378994299191,38.9101601847765,2.28432898886388));
#11267=CARTESIAN_POINT('Ctrl Pts',(47.537899429919,38.9101601847765,2.28432898886389));
#11268=CARTESIAN_POINT('Ctrl Pts',(47.5369318666484,38.9082304179831,2.28728060229702));
#11269=CARTESIAN_POINT('Ctrl Pts',(47.5359829808858,38.9063114473632,2.29024898483066));
#11270=CARTESIAN_POINT('Ctrl Pts',(47.5103321742929,38.8537012755249,2.37256538308168));
#11271=CARTESIAN_POINT('Ctrl Pts',(47.5,38.8134307752649,2.45971883424642));
#11272=CARTESIAN_POINT('Ctrl Pts',(47.5,38.7858156353757,2.5524281532146));
#11273=CARTESIAN_POINT('Origin',(47.5,54.6122755947453,-11.9999999999999));
#11274=CARTESIAN_POINT('Origin',(47.5,54.6122755947453,-11.9999999999999));
#11275=CARTESIAN_POINT('Origin',(37.5,54.6122755947453,-11.9999999999999));
#11276=CARTESIAN_POINT('Origin',(37.5,54.6122755947453,-11.9999999999999));
#11277=CARTESIAN_POINT('Origin',(47.5,39.7674499781695,-26.8448256165756));
#11278=CARTESIAN_POINT('',(47.5,38.7858156353755,-26.5524281532142));
#11279=CARTESIAN_POINT('',(47.5,40.059847441531,-27.8264599593697));
#11280=CARTESIAN_POINT('Origin',(47.5,39.7674499781695,-26.8448256165756));
#11281=CARTESIAN_POINT('',(47.5378994299191,38.9101601847763,-26.2843289888635));
#11282=CARTESIAN_POINT('Ctrl Pts',(47.5,38.7858156353755,-26.5524281532142));
#11283=CARTESIAN_POINT('Ctrl Pts',(47.5,38.8055983895958,-26.4860136545571));
#11284=CARTESIAN_POINT('Ctrl Pts',(47.5053044417601,38.8319740712809,-26.4221125068513));
#11285=CARTESIAN_POINT('Ctrl Pts',(47.5230476022982,38.8786874506599,-26.3347939563902));
#11286=CARTESIAN_POINT('Ctrl Pts',(47.5298073931342,38.8940209364687,-26.309014262892));
#11287=CARTESIAN_POINT('Ctrl Pts',(47.5378994299191,38.9101601847763,-26.2843289888635));
#11288=CARTESIAN_POINT('',(37.462100570081,38.9101601847763,-26.2843289888635));
#11289=CARTESIAN_POINT('',(47.5378994299191,38.9101601847763,-26.2843289888635));
#11290=CARTESIAN_POINT('',(37.5,38.7858156353755,-26.5524281532142));
#11291=CARTESIAN_POINT('Ctrl Pts',(37.462100570081,38.9101601847763,-26.2843289888635));
#11292=CARTESIAN_POINT('Ctrl Pts',(37.463274409961,38.9078190074188,-26.2879098622423));
#11293=CARTESIAN_POINT('Ctrl Pts',(37.464420738878,38.9054937613009,-26.2915153534214));
#11294=CARTESIAN_POINT('Ctrl Pts',(37.4898409184867,38.8530372790542,-26.3739929697886));
#11295=CARTESIAN_POINT('Ctrl Pts',(37.5,38.8131993165768,-26.4604958854362));
#11296=CARTESIAN_POINT('Ctrl Pts',(37.5,38.7858156353755,-26.5524281532142));
#11297=CARTESIAN_POINT('',(37.5,40.059847441531,-27.8264599593697));
#11298=CARTESIAN_POINT('Origin',(37.5,39.7674499781695,-26.8448256165756));
#11299=CARTESIAN_POINT('',(37.462100570081,40.3279466058817,-27.7021154099689));
#11300=CARTESIAN_POINT('Ctrl Pts',(37.5,40.059847441531,-27.8264599593697));
#11301=CARTESIAN_POINT('Ctrl Pts',(37.5,40.1254599686575,-27.8069160868092));
#11302=CARTESIAN_POINT('Ctrl Pts',(37.4948229521316,40.1886351821059,-27.7809329398586));
#11303=CARTESIAN_POINT('Ctrl Pts',(37.4773121076774,40.2761044843057,-27.7344060289472));
#11304=CARTESIAN_POINT('Ctrl Pts',(37.470409170669,40.3026006901669,-27.7186865862431));
#11305=CARTESIAN_POINT('Ctrl Pts',(37.462100570081,40.3279466058817,-27.7021154099689));
#11306=CARTESIAN_POINT('',(47.5378994299191,40.3279466058817,-27.7021154099689));
#11307=CARTESIAN_POINT('',(47.5378994299191,40.3279466058817,-27.7021154099689));
#11308=CARTESIAN_POINT('Ctrl Pts',(47.5378994299191,40.3279466058817,-27.7021154099689));
#11309=CARTESIAN_POINT('Ctrl Pts',(47.5369318666484,40.3249949924486,-27.7040451767622));
#11310=CARTESIAN_POINT('Ctrl Pts',(47.5359829808858,40.3220266099149,-27.7059641473822));
#11311=CARTESIAN_POINT('Ctrl Pts',(47.5103321742929,40.2397102116637,-27.7585743192207));
#11312=CARTESIAN_POINT('Ctrl Pts',(47.5,40.1525567604989,-27.7988448194806));
#11313=CARTESIAN_POINT('Ctrl Pts',(47.5,40.059847441531,-27.8264599593697));
#11314=CARTESIAN_POINT('Origin',(47.5,54.6122755947453,-11.9999999999999));
#11315=CARTESIAN_POINT('Origin',(47.5,54.6122755947453,-11.9999999999999));
#11316=CARTESIAN_POINT('Origin',(37.5,54.6122755947453,-11.9999999999999));
#11317=CARTESIAN_POINT('Origin',(37.5,54.6122755947453,-11.9999999999999));
#11318=CARTESIAN_POINT('Origin',(47.5,69.457101211321,-26.8448256165758));
#11319=CARTESIAN_POINT('',(47.5,69.1647037479595,-27.8264599593698));
#11320=CARTESIAN_POINT('',(47.5,70.4387355541151,-26.5524281532143));
#11321=CARTESIAN_POINT('Origin',(47.5,69.457101211321,-26.8448256165758));
#11322=CARTESIAN_POINT('',(47.5378994299191,68.8966045836088,-27.702115409969));
#11323=CARTESIAN_POINT('Ctrl Pts',(47.5,69.1647037479595,-27.8264599593698));
#11324=CARTESIAN_POINT('Ctrl Pts',(47.5,69.0982892493024,-27.8066772051495));
#11325=CARTESIAN_POINT('Ctrl Pts',(47.5053044417601,69.0343881015963,-27.7803015234644));
#11326=CARTESIAN_POINT('Ctrl Pts',(47.5230476022983,68.9470695511352,-27.7335881440852));
#11327=CARTESIAN_POINT('Ctrl Pts',(47.5298073931342,68.9212898576372,-27.7182546582765));
#11328=CARTESIAN_POINT('Ctrl Pts',(47.5378994299191,68.8966045836088,-27.702115409969));
#11329=CARTESIAN_POINT('',(37.462100570081,68.8966045836088,-27.702115409969));
#11330=CARTESIAN_POINT('',(47.5378994299191,68.8966045836088,-27.702115409969));
#11331=CARTESIAN_POINT('',(37.5,69.1647037479595,-27.8264599593698));
#11332=CARTESIAN_POINT('Ctrl Pts',(37.462100570081,68.8966045836088,-27.702115409969));
#11333=CARTESIAN_POINT('Ctrl Pts',(37.4632744099607,68.900185456987,-27.704456587326));
#11334=CARTESIAN_POINT('Ctrl Pts',(37.4644207388776,68.9037909481654,-27.7067818334436));
#11335=CARTESIAN_POINT('Ctrl Pts',(37.4898409184865,68.9862685645324,-27.7592383156903));
#11336=CARTESIAN_POINT('Ctrl Pts',(37.5,69.0727714801806,-27.7990762781682));
#11337=CARTESIAN_POINT('Ctrl Pts',(37.5,69.1647037479595,-27.8264599593698));
#11338=CARTESIAN_POINT('',(37.5,70.4387355541151,-26.5524281532143));
#11339=CARTESIAN_POINT('Origin',(37.5,69.457101211321,-26.8448256165758));
#11340=CARTESIAN_POINT('',(37.462100570081,70.3143910047142,-26.2843289888636));
#11341=CARTESIAN_POINT('Ctrl Pts',(37.5,70.4387355541151,-26.5524281532143));
#11342=CARTESIAN_POINT('Ctrl Pts',(37.5,70.4191916815546,-26.4868156260878));
#11343=CARTESIAN_POINT('Ctrl Pts',(37.4948229521316,70.3932085346039,-26.4236404126394));
#11344=CARTESIAN_POINT('Ctrl Pts',(37.4773121076774,70.3466816236925,-26.3361711104396));
#11345=CARTESIAN_POINT('Ctrl Pts',(37.470409170669,70.3309621809885,-26.3096749045784));
#11346=CARTESIAN_POINT('Ctrl Pts',(37.462100570081,70.3143910047142,-26.2843289888636));
#11347=CARTESIAN_POINT('',(47.5378994299191,70.3143910047142,-26.2843289888636));
#11348=CARTESIAN_POINT('',(47.5378994299191,70.3143910047142,-26.2843289888636));
#11349=CARTESIAN_POINT('Ctrl Pts',(47.5378994299191,70.3143910047142,-26.2843289888636));
#11350=CARTESIAN_POINT('Ctrl Pts',(47.5369318666484,70.3163207715076,-26.2872806022967));
#11351=CARTESIAN_POINT('Ctrl Pts',(47.5359829808858,70.3182397421275,-26.2902489848303));
#11352=CARTESIAN_POINT('Ctrl Pts',(47.510332174293,70.3708499139657,-26.3725653830812));
#11353=CARTESIAN_POINT('Ctrl Pts',(47.5,70.4111204142258,-26.4597188342459));
#11354=CARTESIAN_POINT('Ctrl Pts',(47.5,70.4387355541151,-26.5524281532143));
#11355=CARTESIAN_POINT('Origin',(47.5,54.6122755947453,-11.9999999999999));
#11356=CARTESIAN_POINT('Origin',(47.5,54.6122755947453,-11.9999999999999));
#11357=CARTESIAN_POINT('Origin',(37.5,54.6122755947453,-11.9999999999999));
#11358=CARTESIAN_POINT('Origin',(37.5,54.6122755947453,-11.9999999999999));
#11359=CARTESIAN_POINT('Origin',(47.5,71.1513780613053,-25.7371063037536));
#11360=CARTESIAN_POINT('Ctrl Pts',(37.462100570081,70.3143910047142,-26.2843289888636));
#11361=CARTESIAN_POINT('Ctrl Pts',(37.4310083838417,70.2523788651895,-26.1894802928099));
#11362=CARTESIAN_POINT('Ctrl Pts',(37.3828779782928,70.2100019065445,-26.0896111315555));
#11363=CARTESIAN_POINT('Ctrl Pts',(37.2450318222992,70.1490670949059,-25.8572144843843));
#11364=CARTESIAN_POINT('Ctrl Pts',(37.1423703640169,70.1421609442904,-25.7182913573665));
#11365=CARTESIAN_POINT('Ctrl Pts',(36.8667626333183,70.1911329104162,-25.4052183599692));
#11366=CARTESIAN_POINT('Ctrl Pts',(36.6872103877121,70.2659230524829,-25.2392991703043));
#11367=CARTESIAN_POINT('Ctrl Pts',(36.5029780432812,70.3802619217331,-25.1004101333781));
#11368=CARTESIAN_POINT('Ctrl Pts',(36.5014890205775,70.3811884825665,-25.0992896162488));
#11369=CARTESIAN_POINT('Ctrl Pts',(36.5,70.3821174814653,-25.0981711268349));
#11370=CARTESIAN_POINT('Ctrl Pts',(47.5378994299191,70.3143910047142,-26.2843289888636));
#11371=CARTESIAN_POINT('Ctrl Pts',(47.568991616158,70.2523788651901,-26.1894802928108));
#11372=CARTESIAN_POINT('Ctrl Pts',(47.6171220217063,70.2100019065453,-26.0896111315574));
#11373=CARTESIAN_POINT('Ctrl Pts',(47.7549681776988,70.1490670949063,-25.8572144843871));
#11374=CARTESIAN_POINT('Ctrl Pts',(47.8576296359807,70.1421609442904,-25.7182913573697));
#11375=CARTESIAN_POINT('Ctrl Pts',(48.1332373667109,70.1911329104208,-25.4052183599355));
#11376=CARTESIAN_POINT('Ctrl Pts',(48.3127896123394,70.2659230524989,-25.2392991702846));
#11377=CARTESIAN_POINT('Ctrl Pts',(48.4970219567185,70.3802619217334,-25.1004101333777));
#11378=CARTESIAN_POINT('Ctrl Pts',(48.4985109794227,70.3811884825666,-25.0992896162486));
#11379=CARTESIAN_POINT('Ctrl Pts',(48.5,70.3821174814653,-25.0981711268349));
#11380=CARTESIAN_POINT('Origin',(48.5,54.6122755947453,-11.9999999999999));
#11381=CARTESIAN_POINT('Ctrl Pts',(47.5378994299191,68.8966045836088,-27.702115409969));
#11382=CARTESIAN_POINT('Ctrl Pts',(47.5689916161593,68.8017558875521,-27.6401032704423));
#11383=CARTESIAN_POINT('Ctrl Pts',(47.6171220217102,68.7018867262945,-27.5977263117966));
#11384=CARTESIAN_POINT('Ctrl Pts',(47.7549681777078,68.4694900791192,-27.5367915001594));
#11385=CARTESIAN_POINT('Ctrl Pts',(47.857629635992,68.3305669521004,-27.5298853495452));
#11386=CARTESIAN_POINT('Ctrl Pts',(48.1332373665661,68.0174939548474,-27.5788573156524));
#11387=CARTESIAN_POINT('Ctrl Pts',(48.3127896120915,67.8515747651331,-27.6536474576698));
#11388=CARTESIAN_POINT('Ctrl Pts',(48.4970219567174,67.7126857281265,-27.7679863269852));
#11389=CARTESIAN_POINT('Ctrl Pts',(48.4985109794222,67.7115652109942,-27.7689128878211));
#11390=CARTESIAN_POINT('Ctrl Pts',(48.5,67.71044672158,-27.7698418867201));
#11391=CARTESIAN_POINT('Origin',(36.5,54.6122755947453,-11.9999999999999));
#11392=CARTESIAN_POINT('Ctrl Pts',(37.462100570081,68.8966045836088,-27.702115409969));
#11393=CARTESIAN_POINT('Ctrl Pts',(37.4310083838413,68.8017558875538,-27.6401032704434));
#11394=CARTESIAN_POINT('Ctrl Pts',(37.3828779782915,68.701886726298,-27.5977263117981));
#11395=CARTESIAN_POINT('Ctrl Pts',(37.245031822296,68.4694900791247,-27.5367915001601));
#11396=CARTESIAN_POINT('Ctrl Pts',(37.1423703640128,68.3305669521065,-27.5298853495452));
#11397=CARTESIAN_POINT('Ctrl Pts',(36.8667626333661,68.0174939547694,-27.5788573156634));
#11398=CARTESIAN_POINT('Ctrl Pts',(36.6872103877933,67.8515747650841,-27.6536474577095));
#11399=CARTESIAN_POINT('Ctrl Pts',(36.5029780432822,67.7126857281249,-27.7679863269865));
#11400=CARTESIAN_POINT('Ctrl Pts',(36.5014890205769,67.7115652109935,-27.7689128878217));
#11401=CARTESIAN_POINT('Ctrl Pts',(36.5,67.71044672158,-27.7698418867201));
#11402=CARTESIAN_POINT('Origin',(50.,68.3493818984988,-28.5391024665601));
#11403=CARTESIAN_POINT('Origin',(47.5,40.8751692909917,-28.5391024665599));
#11404=CARTESIAN_POINT('Ctrl Pts',(37.462100570081,40.3279466058817,-27.7021154099689));
#11405=CARTESIAN_POINT('Ctrl Pts',(37.4310083838416,40.4227953019356,-27.640103270444));
#11406=CARTESIAN_POINT('Ctrl Pts',(37.3828779782926,40.5226644631903,-27.5977263117989));
#11407=CARTESIAN_POINT('Ctrl Pts',(37.2450318222986,40.755061110362,-27.5367915001605));
#11408=CARTESIAN_POINT('Ctrl Pts',(37.1423703640161,40.8939842373798,-27.529885349545));
#11409=CARTESIAN_POINT('Ctrl Pts',(36.8667626333263,41.2070572347668,-27.5788573156696));
#11410=CARTESIAN_POINT('Ctrl Pts',(36.6872103877253,41.3729764244348,-27.6536474577325));
#11411=CARTESIAN_POINT('Ctrl Pts',(36.5029780432813,41.511865461367,-27.7679863269875));
#11412=CARTESIAN_POINT('Ctrl Pts',(36.5014890205774,41.5129859784966,-27.7689128878212));
#11413=CARTESIAN_POINT('Ctrl Pts',(36.5,41.5141044679104,-27.7698418867199));
#11414=CARTESIAN_POINT('Ctrl Pts',(47.5378994299191,40.3279466058817,-27.7021154099689));
#11415=CARTESIAN_POINT('Ctrl Pts',(47.5689916161584,40.4227953019356,-27.640103270444));
#11416=CARTESIAN_POINT('Ctrl Pts',(47.6171220217074,40.5226644631902,-27.597726311799));
#11417=CARTESIAN_POINT('Ctrl Pts',(47.7549681777013,40.7550611103619,-27.5367915001605));
#11418=CARTESIAN_POINT('Ctrl Pts',(47.8576296359839,40.8939842373797,-27.5298853495451));
#11419=CARTESIAN_POINT('Ctrl Pts',(48.1332373666762,41.2070572347697,-27.57885731567));
#11420=CARTESIAN_POINT('Ctrl Pts',(48.3127896122781,41.3729764244373,-27.6536474577346));
#11421=CARTESIAN_POINT('Ctrl Pts',(48.497021956718,41.5118654613665,-27.7679863269871));
#11422=CARTESIAN_POINT('Ctrl Pts',(48.4985109794233,41.5129859784971,-27.7689128878216));
#11423=CARTESIAN_POINT('Ctrl Pts',(48.5,41.5141044679105,-27.7698418867199));
#11424=CARTESIAN_POINT('Origin',(48.5,54.6122755947453,-11.9999999999999));
#11425=CARTESIAN_POINT('Ctrl Pts',(47.5378994299191,38.9101601847763,-26.2843289888635));
#11426=CARTESIAN_POINT('Ctrl Pts',(47.5689916161584,38.9721723243012,-26.1894802928096));
#11427=CARTESIAN_POINT('Ctrl Pts',(47.6171220217074,39.0145492829462,-26.0896111315549));
#11428=CARTESIAN_POINT('Ctrl Pts',(47.7549681777013,39.0754840945847,-25.8572144843834));
#11429=CARTESIAN_POINT('Ctrl Pts',(47.8576296359838,39.0823902452002,-25.7182913573655));
#11430=CARTESIAN_POINT('Ctrl Pts',(48.1332373666738,39.0334182790756,-25.4052183599782));
#11431=CARTESIAN_POINT('Ctrl Pts',(48.3127896122749,38.9586281370126,-25.2392991703103));
#11432=CARTESIAN_POINT('Ctrl Pts',(48.497021956719,38.8442892677574,-25.1004101333779));
#11433=CARTESIAN_POINT('Ctrl Pts',(48.4985109794223,38.8433627069242,-25.0992896162488));
#11434=CARTESIAN_POINT('Ctrl Pts',(48.5,38.8424337080252,-25.0981711268347));
#11435=CARTESIAN_POINT('Origin',(36.5,54.6122755947453,-11.9999999999999));
#11436=CARTESIAN_POINT('Ctrl Pts',(37.462100570081,38.9101601847763,-26.2843289888635));
#11437=CARTESIAN_POINT('Ctrl Pts',(37.4310083838421,38.9721723243003,-26.1894802928109));
#11438=CARTESIAN_POINT('Ctrl Pts',(37.3828779782939,39.0145492829451,-26.0896111315576));
#11439=CARTESIAN_POINT('Ctrl Pts',(37.2450318223019,39.075484094584,-25.8572144843881));
#11440=CARTESIAN_POINT('Ctrl Pts',(37.1423703640203,39.0823902452002,-25.7182913573708));
#11441=CARTESIAN_POINT('Ctrl Pts',(36.8667626332853,39.0334182790692,-25.4052183599309));
#11442=CARTESIAN_POINT('Ctrl Pts',(36.6872103876556,38.9586281369882,-25.2392991702806));
#11443=CARTESIAN_POINT('Ctrl Pts',(36.502978043283,38.844289267758,-25.1004101333787));
#11444=CARTESIAN_POINT('Ctrl Pts',(36.5014890205765,38.8433627069234,-25.0992896162479));
#11445=CARTESIAN_POINT('Ctrl Pts',(36.5,38.8424337080252,-25.0981711268347));
#11446=CARTESIAN_POINT('Origin',(50.,38.0731731281852,-25.7371063037535));
#11447=CARTESIAN_POINT('Origin',(47.5,38.0731731281855,1.73710630375391));
#11448=CARTESIAN_POINT('Ctrl Pts',(37.462100570081,38.9101601847765,2.2843289888639));
#11449=CARTESIAN_POINT('Ctrl Pts',(37.4310083838418,38.9721723243011,2.1894802928104));
#11450=CARTESIAN_POINT('Ctrl Pts',(37.382877978293,39.0145492829461,2.0896111315562));
#11451=CARTESIAN_POINT('Ctrl Pts',(37.2450318222997,39.0754840945847,1.85721448438531));
#11452=CARTESIAN_POINT('Ctrl Pts',(37.1423703640175,39.0823902452004,1.71829135736766));
#11453=CARTESIAN_POINT('Ctrl Pts',(36.8667626333158,39.0334182790742,1.40521835996645));
#11454=CARTESIAN_POINT('Ctrl Pts',(36.6872103877081,38.9586281370059,1.23929917030242));
#11455=CARTESIAN_POINT('Ctrl Pts',(36.5029780432818,38.844289267758,1.10041013337881));
#11456=CARTESIAN_POINT('Ctrl Pts',(36.5014890205776,38.8433627069243,1.09928961624914));
#11457=CARTESIAN_POINT('Ctrl Pts',(36.5,38.8424337080254,1.09817112683512));
#11458=CARTESIAN_POINT('Ctrl Pts',(47.5378994299191,38.9101601847765,2.2843289888639));
#11459=CARTESIAN_POINT('Ctrl Pts',(47.5689916161585,38.9721723243016,2.18948029280961));
#11460=CARTESIAN_POINT('Ctrl Pts',(47.6171220217078,39.0145492829468,2.08961113155459));
#11461=CARTESIAN_POINT('Ctrl Pts',(47.7549681777024,39.0754840945851,1.85721448438222));
#11462=CARTESIAN_POINT('Ctrl Pts',(47.8576296359852,39.0823902452003,1.71829135736426));
#11463=CARTESIAN_POINT('Ctrl Pts',(48.1332373666565,39.0334182790786,1.40521835999846));
#11464=CARTESIAN_POINT('Ctrl Pts',(48.3127896122453,38.9586281370227,1.23929917032299));
#11465=CARTESIAN_POINT('Ctrl Pts',(48.4970219567186,38.8442892677582,1.10041013337901));
#11466=CARTESIAN_POINT('Ctrl Pts',(48.4985109794219,38.8433627069246,1.09928961624948));
#11467=CARTESIAN_POINT('Ctrl Pts',(48.5,38.8424337080254,1.09817112683513));
#11468=CARTESIAN_POINT('Origin',(48.5,54.6122755947453,-11.9999999999999));
#11469=CARTESIAN_POINT('Ctrl Pts',(47.5378994299191,40.3279466058819,3.70211540996925));
#11470=CARTESIAN_POINT('Ctrl Pts',(47.5689916161576,40.4227953019335,3.64010327044594));
#11471=CARTESIAN_POINT('Ctrl Pts',(47.6171220217051,40.5226644631856,3.59772631180138));
#11472=CARTESIAN_POINT('Ctrl Pts',(47.7549681776959,40.7550611103542,3.53679150016188));
#11473=CARTESIAN_POINT('Ctrl Pts',(47.857629635977,40.8939842373711,3.5298853495454));
#11474=CARTESIAN_POINT('Ctrl Pts',(48.1332373667501,41.2070572348553,3.57885731568198));
#11475=CARTESIAN_POINT('Ctrl Pts',(48.3127896124051,41.3729764244901,3.65364745777795));
#11476=CARTESIAN_POINT('Ctrl Pts',(48.4970219567172,41.5118654613675,3.76798632698816));
#11477=CARTESIAN_POINT('Ctrl Pts',(48.4985109794234,41.5129859784975,3.76891288782207));
#11478=CARTESIAN_POINT('Ctrl Pts',(48.5,41.5141044679107,3.76984188672031));
#11479=CARTESIAN_POINT('Origin',(36.5,54.6122755947453,-11.9999999999999));
#11480=CARTESIAN_POINT('Ctrl Pts',(37.462100570081,40.3279466058819,3.70211540996925));
#11481=CARTESIAN_POINT('Ctrl Pts',(37.4310083838421,40.4227953019343,3.64010327044543));
#11482=CARTESIAN_POINT('Ctrl Pts',(37.3828779782942,40.5226644631872,3.5977263118007));
#11483=CARTESIAN_POINT('Ctrl Pts',(37.2450318223022,40.755061110357,3.53679150016149));
#11484=CARTESIAN_POINT('Ctrl Pts',(37.1423703640206,40.8939842373742,3.52988534954544));
#11485=CARTESIAN_POINT('Ctrl Pts',(36.8667626332747,41.2070572348267,3.57885731567809));
#11486=CARTESIAN_POINT('Ctrl Pts',(36.6872103876371,41.3729764244722,3.65364745776331));
#11487=CARTESIAN_POINT('Ctrl Pts',(36.5029780432816,41.511865461368,3.76798632698854));
#11488=CARTESIAN_POINT('Ctrl Pts',(36.5014890205776,41.5129859784967,3.76891288782145));
#11489=CARTESIAN_POINT('Ctrl Pts',(36.5,41.5141044679107,3.76984188672031));
#11490=CARTESIAN_POINT('Origin',(50.,40.8751692909919,4.53910246656033));
#11491=CARTESIAN_POINT('Origin',(36.,54.6122755947453,-11.9999999999999));
#11492=CARTESIAN_POINT('Origin',(36.,54.6122755947453,7.50000000000008));
#11493=CARTESIAN_POINT('Origin',(49.,54.6122755947453,-11.9999999999999));
#11494=CARTESIAN_POINT('Origin',(49.,54.6122755947453,7.50000000000009));
#11495=CARTESIAN_POINT('Origin',(35.,54.6122755947453,-11.9999999999999));
#11496=CARTESIAN_POINT('',(35.,54.6122755947453,5.50000000000008));
#11497=CARTESIAN_POINT('',(0.,0.,0.));
#11498=CARTESIAN_POINT('',(0.,0.,0.));
#11499=CARTESIAN_POINT('Origin',(3.21444260098502E-12,109.,121.5));
#11500=CARTESIAN_POINT('',(-11.2583302491955,102.499999999999,121.5));
#11501=CARTESIAN_POINT('',(11.2583302492019,115.500000000001,121.5));
#11502=CARTESIAN_POINT('Origin',(3.21444260098502E-12,109.,121.5));
#11503=CARTESIAN_POINT('',(9.52627944163062,114.499999999999,121.5));
#11504=CARTESIAN_POINT('',(11.2583302492019,115.500000000001,121.5));
#11505=CARTESIAN_POINT('',(-9.52627944162417,103.500000000001,121.5));
#11506=CARTESIAN_POINT('Origin',(3.21444260098502E-12,109.,121.5));
#11507=CARTESIAN_POINT('',(-9.52627944162417,103.500000000001,121.5));
#11508=CARTESIAN_POINT('Origin',(11.2583302492011,115.500000000001,60.4999999999998));
#11509=CARTESIAN_POINT('',(9.52627944162984,114.499999999999,65.5));
#11510=CARTESIAN_POINT('',(11.2583302491965,115.499999999998,65.5));
#11511=CARTESIAN_POINT('',(9.52627944162984,114.499999999999,65.5));
#11512=CARTESIAN_POINT('',(9.52627944162984,114.499999999999,65.5));
#11513=CARTESIAN_POINT('',(11.2583302492012,115.500000000001,65.5));
#11514=CARTESIAN_POINT('Origin',(2.36789754470834E-12,109.,60.5));
#11515=CARTESIAN_POINT('',(-9.52627944162487,103.500000000001,65.5));
#11516=CARTESIAN_POINT('Origin',(2.43784159525973E-12,109.,65.5));
#11517=CARTESIAN_POINT('',(-9.52627944162496,103.500000000001,65.5));
#11518=CARTESIAN_POINT('Origin',(-9.52627944162501,103.500000000001,60.5000000000001));
#11519=CARTESIAN_POINT('',(-11.2583302491953,102.5,65.5));
#11520=CARTESIAN_POINT('',(-11.2583302491953,102.5,65.5));
#11521=CARTESIAN_POINT('',(-11.2583302491962,102.499999999999,65.5));
#11522=CARTESIAN_POINT('Origin',(2.36789754470834E-12,109.,60.5));
#11523=CARTESIAN_POINT('Origin',(4.79810263127257E-15,109.,65.5));
#11524=CARTESIAN_POINT('Origin',(4.79810263127257E-15,109.,65.5));
#11525=CARTESIAN_POINT('Origin',(-115.614391405224,109.,-78.7499999999976));
#11526=CARTESIAN_POINT('',(-109.985226280625,102.499999999999,-88.4999999999985));
#11527=CARTESIAN_POINT('',(-121.243556529823,115.500000000001,-68.9999999999967));
#11528=CARTESIAN_POINT('Origin',(-115.614391405224,109.,-78.7499999999976));
#11529=CARTESIAN_POINT('',(-120.377531126037,114.499999999999,-70.4999999999988));
#11530=CARTESIAN_POINT('',(-121.243556529823,115.500000000001,-68.9999999999967));
#11531=CARTESIAN_POINT('',(-110.85125168441,103.500000000001,-86.9999999999964));
#11532=CARTESIAN_POINT('Origin',(-115.614391405224,109.,-78.7499999999976));
#11533=CARTESIAN_POINT('',(-110.85125168441,103.500000000001,-86.9999999999964));
#11534=CARTESIAN_POINT('Origin',(-68.416006898972,115.500000000001,-38.4999999999972));
#11535=CARTESIAN_POINT('',(-71.8801085141086,114.499999999999,-42.4999999999993));
#11536=CARTESIAN_POINT('',(-72.7461339178932,115.499999999999,-40.9999999999989));
#11537=CARTESIAN_POINT('',(-71.8801085141086,114.499999999999,-42.4999999999993));
#11538=CARTESIAN_POINT('',(-71.8801085141086,114.499999999999,-42.4999999999993));
#11539=CARTESIAN_POINT('',(-72.7461339178942,115.500000000001,-40.9999999999972));
#11540=CARTESIAN_POINT('Origin',(-62.7868417743727,109.,-48.2499999999981));
#11541=CARTESIAN_POINT('',(-62.3538290724813,103.500000000001,-58.9999999999969));
#11542=CARTESIAN_POINT('Origin',(-67.116968793295,109.,-50.7499999999981));
#11543=CARTESIAN_POINT('',(-62.3538290724813,103.500000000001,-58.9999999999969));
#11544=CARTESIAN_POINT('Origin',(-58.0237020535591,103.500000000001,-56.4999999999969));
#11545=CARTESIAN_POINT('',(-61.4878036686957,102.499999999999,-60.499999999999));
#11546=CARTESIAN_POINT('',(-61.4878036686957,102.499999999999,-60.499999999999));
#11547=CARTESIAN_POINT('',(-61.4878036686957,102.499999999999,-60.499999999999));
#11548=CARTESIAN_POINT('Origin',(-62.7868417743727,109.,-48.2499999999981));
#11549=CARTESIAN_POINT('Origin',(-67.1169687932943,109.,-50.7499999999993));
#11550=CARTESIAN_POINT('Origin',(-67.1169687932943,109.,-50.7499999999993));
#11551=CARTESIAN_POINT('Origin',(115.614391405221,109.,-78.7500000000032));
#11552=CARTESIAN_POINT('',(121.24355652982,102.499999999999,-69.0000000000025));
#11553=CARTESIAN_POINT('',(109.985226280621,115.500000000001,-88.500000000004));
#11554=CARTESIAN_POINT('Origin',(115.614391405221,109.,-78.7500000000032));
#11555=CARTESIAN_POINT('',(110.851251684407,114.499999999999,-87.0000000000019));
#11556=CARTESIAN_POINT('',(109.985226280621,115.500000000001,-88.500000000004));
#11557=CARTESIAN_POINT('',(120.377531126034,103.500000000001,-70.5000000000045));
#11558=CARTESIAN_POINT('Origin',(115.614391405221,109.,-78.7500000000032));
#11559=CARTESIAN_POINT('',(120.377531126034,103.500000000001,-70.5000000000045));
#11560=CARTESIAN_POINT('Origin',(57.1576766497708,115.500000000001,-58.000000000003));
#11561=CARTESIAN_POINT('',(62.3538290724788,114.499999999999,-59.0000000000011));
#11562=CARTESIAN_POINT('',(61.4878036686952,115.499999999998,-60.4999999999996));
#11563=CARTESIAN_POINT('',(62.3538290724788,114.499999999999,-59.0000000000011));
#11564=CARTESIAN_POINT('',(62.3538290724788,114.499999999999,-59.0000000000011));
#11565=CARTESIAN_POINT('',(61.4878036686932,115.500000000001,-60.5000000000032));
#11566=CARTESIAN_POINT('Origin',(62.7868417743704,109.,-48.2500000000022));
#11567=CARTESIAN_POINT('',(71.8801085141063,103.500000000001,-42.5000000000036));
#11568=CARTESIAN_POINT('Origin',(67.1169687932926,109.,-50.7500000000023));
#11569=CARTESIAN_POINT('',(71.8801085141063,103.500000000001,-42.5000000000036));
#11570=CARTESIAN_POINT('Origin',(67.5499814951842,103.500000000001,-40.0000000000036));
#11571=CARTESIAN_POINT('',(72.7461339178917,102.5,-41.0000000000018));
#11572=CARTESIAN_POINT('',(72.7461339178918,102.5,-41.0000000000018));
#11573=CARTESIAN_POINT('',(72.7461339178919,102.499999999999,-41.0000000000015));
#11574=CARTESIAN_POINT('Origin',(62.7868417743704,109.,-48.2500000000022));
#11575=CARTESIAN_POINT('Origin',(67.1169687932938,109.,-50.7500000000002));
#11576=CARTESIAN_POINT('Origin',(67.1169687932938,109.,-50.7500000000002));
#11577=CARTESIAN_POINT('Origin',(-67.1169687932943,109.,-50.7499999999992));
#11578=CARTESIAN_POINT('',(-64.7881663535555,123.258566435188,-54.7836041464173));
#11579=CARTESIAN_POINT('',(-61.3240647384177,123.258566435188,-52.7836041464173));
#11580=CARTESIAN_POINT('',(-64.7881663535555,123.258566435188,-54.7836041464173));
#11581=CARTESIAN_POINT('',(-74.5423344792075,106.889128681836,-37.8888893672188));
#11582=CARTESIAN_POINT('Origin',(-67.1169687932943,109.,-50.7499999999992));
#11583=CARTESIAN_POINT('',(-71.0782328640697,106.889128681836,-35.8888893672189));
#11584=CARTESIAN_POINT('',(-74.5423344792075,106.889128681836,-37.8888893672188));
#11585=CARTESIAN_POINT('Origin',(-63.6528671781565,109.,-48.7499999999993));
#11586=CARTESIAN_POINT('Origin',(-67.1169687932943,109.,-50.7499999999992));
#11587=CARTESIAN_POINT('',(-60.8542184280248,122.916546291862,-53.5974018277667));
#11588=CARTESIAN_POINT('',(-64.3183200431626,122.916546291862,-55.5974018277666));
#11589=CARTESIAN_POINT('',(-64.3183200431626,122.916546291862,-55.5974018277666));
#11590=CARTESIAN_POINT('',(-58.6431280208156,97.837112635988,-57.4271227531812));
#11591=CARTESIAN_POINT('Origin',(-63.6528671781565,109.,-48.7499999999993));
#11592=CARTESIAN_POINT('',(-62.1072296359534,97.837112635988,-59.4271227531812));
#11593=CARTESIAN_POINT('',(-62.1072296359534,97.837112635988,-59.4271227531812));
#11594=CARTESIAN_POINT('Origin',(-67.1169687932943,109.,-50.7499999999992));
#11595=CARTESIAN_POINT('Origin',(-67.1169687932943,109.,-50.7499999999992));
#11596=CARTESIAN_POINT('',(-59.0261502423751,97.1943250263015,-56.7637088050123));
#11597=CARTESIAN_POINT('',(-62.4902518575129,97.1943250263015,-58.7637088050122));
#11598=CARTESIAN_POINT('',(-62.4902518575129,97.1943250263015,-58.7637088050122));
#11599=CARTESIAN_POINT('',(-70.9914087752362,105.904320928824,-36.0392731003993));
#11600=CARTESIAN_POINT('Origin',(-63.6528671781565,109.,-48.7499999999993));
#11601=CARTESIAN_POINT('',(-74.455510390374,105.904320928824,-38.0392731003992));
#11602=CARTESIAN_POINT('',(-74.455510390374,105.904320928824,-38.0392731003992));
#11603=CARTESIAN_POINT('Origin',(-67.1169687932943,109.,-50.7499999999992));
#11604=CARTESIAN_POINT('Origin',(-67.1169687932943,109.,-50.7499999999992));
#11605=CARTESIAN_POINT('',(-64.9661511107924,122.280548232157,-54.4753255039102));
#11606=CARTESIAN_POINT('',(-64.7881663535555,123.258566435188,-54.7836041464173));
#11607=CARTESIAN_POINT('',(-64.4963048003994,121.938528088831,-55.2891231852596));
#11608=CARTESIAN_POINT('',(-64.4963048003994,121.938528088831,-55.2891231852596));
#11609=CARTESIAN_POINT('',(-64.4963048003994,121.938528088831,-55.2891231852596));
#11610=CARTESIAN_POINT('',(-62.4417315619291,98.6344003800105,-58.8477484221616));
#11611=CARTESIAN_POINT('',(-62.1072296359534,97.837112635988,-59.4271227531812));
#11612=CARTESIAN_POINT('',(-62.8247537834885,97.9916127703239,-58.1843344739927));
#11613=CARTESIAN_POINT('',(-62.8247537834885,97.9916127703239,-58.1843344739927));
#11614=CARTESIAN_POINT('',(-62.8247537834886,97.9916127703239,-58.1843344739927));
#11615=CARTESIAN_POINT('',(-73.9430237071614,106.085051387833,-38.9269260739259));
#11616=CARTESIAN_POINT('',(-74.455510390374,105.904320928824,-38.0392731003992));
#11617=CARTESIAN_POINT('',(-74.0298477959949,107.069859140845,-38.7765423407454));
#11618=CARTESIAN_POINT('',(-74.0298477959949,107.069859140845,-38.7765423407454));
#11619=CARTESIAN_POINT('',(-74.0298477959949,107.069859140845,-38.7765423407454));
#11620=CARTESIAN_POINT('',(-60.6169687932938,109.,-62.0083302491979));
#11621=CARTESIAN_POINT('Origin',(-67.1169687932943,109.,-50.7499999999993));
#11622=CARTESIAN_POINT('Origin',(67.1169687932938,109.,-50.7500000000002));
#11623=CARTESIAN_POINT('',(69.4457712330326,123.258566435188,-46.7163958535822));
#11624=CARTESIAN_POINT('',(65.9816696178948,123.258566435188,-44.7163958535822));
#11625=CARTESIAN_POINT('',(69.4457712330326,123.258566435188,-46.7163958535822));
#11626=CARTESIAN_POINT('',(59.6916031073804,106.889128681836,-63.6111106327805));
#11627=CARTESIAN_POINT('Origin',(67.1169687932938,109.,-50.7500000000002));
#11628=CARTESIAN_POINT('',(56.2275014922427,106.889128681836,-61.6111106327805));
#11629=CARTESIAN_POINT('',(59.6916031073804,106.889128681836,-63.6111106327805));
#11630=CARTESIAN_POINT('Origin',(63.652867178156,109.,-48.7500000000002));
#11631=CARTESIAN_POINT('Origin',(67.1169687932938,109.,-50.7500000000002));
#11632=CARTESIAN_POINT('',(66.4515159282878,122.916546291862,-43.9025981722328));
#11633=CARTESIAN_POINT('',(69.9156175434256,122.916546291862,-45.9025981722328));
#11634=CARTESIAN_POINT('',(69.9156175434256,122.916546291862,-45.9025981722328));
#11635=CARTESIAN_POINT('',(68.662606335497,97.837112635988,-40.0728772468183));
#11636=CARTESIAN_POINT('Origin',(63.652867178156,109.,-48.7500000000002));
#11637=CARTESIAN_POINT('',(72.1267079506348,97.837112635988,-42.0728772468184));
#11638=CARTESIAN_POINT('',(72.1267079506348,97.837112635988,-42.0728772468184));
#11639=CARTESIAN_POINT('Origin',(67.1169687932938,109.,-50.7500000000002));
#11640=CARTESIAN_POINT('Origin',(67.1169687932938,109.,-50.7500000000002));
#11641=CARTESIAN_POINT('',(68.2795841139375,97.1943250263015,-40.7362911949873));
#11642=CARTESIAN_POINT('',(71.7436857290753,97.1943250263015,-42.7362911949873));
#11643=CARTESIAN_POINT('',(71.7436857290753,97.1943250263015,-42.7362911949873));
#11644=CARTESIAN_POINT('',(56.3143255810761,105.904320928824,-61.4607268996001));
#11645=CARTESIAN_POINT('Origin',(63.652867178156,109.,-48.7500000000002));
#11646=CARTESIAN_POINT('',(59.7784271962139,105.904320928824,-63.4607268996001));
#11647=CARTESIAN_POINT('',(59.7784271962139,105.904320928824,-63.4607268996001));
#11648=CARTESIAN_POINT('Origin',(67.1169687932938,109.,-50.7500000000002));
#11649=CARTESIAN_POINT('Origin',(67.1169687932938,109.,-50.7500000000002));
#11650=CARTESIAN_POINT('',(69.2677864757957,122.280548232157,-47.0246744960893));
#11651=CARTESIAN_POINT('',(69.4457712330326,123.258566435188,-46.7163958535822));
#11652=CARTESIAN_POINT('',(69.7376327861887,121.938528088831,-46.2108768147398));
#11653=CARTESIAN_POINT('',(69.7376327861887,121.938528088831,-46.2108768147398));
#11654=CARTESIAN_POINT('',(69.7376327861887,121.938528088831,-46.2108768147399));
#11655=CARTESIAN_POINT('',(71.7922060246591,98.6344003800105,-42.6522515778379));
#11656=CARTESIAN_POINT('',(72.1267079506348,97.837112635988,-42.0728772468184));
#11657=CARTESIAN_POINT('',(71.4091838030996,97.991612770324,-43.3156655260068));
#11658=CARTESIAN_POINT('',(71.4091838030996,97.991612770324,-43.3156655260068));
#11659=CARTESIAN_POINT('',(71.4091838030996,97.9916127703239,-43.3156655260069));
#11660=CARTESIAN_POINT('',(60.2909138794264,106.085051387833,-62.5730739260735));
#11661=CARTESIAN_POINT('',(59.7784271962139,105.904320928824,-63.4607268996001));
#11662=CARTESIAN_POINT('',(60.204089790593,107.069859140845,-62.7234576592539));
#11663=CARTESIAN_POINT('',(60.204089790593,107.069859140845,-62.7234576592539));
#11664=CARTESIAN_POINT('',(60.2040897905929,107.069859140845,-62.7234576592539));
#11665=CARTESIAN_POINT('',(73.6169687932943,109.,-39.4916697508016));
#11666=CARTESIAN_POINT('Origin',(67.1169687932938,109.,-50.7500000000002));
#11667=CARTESIAN_POINT('Origin',(4.79810263127257E-15,109.,65.5));
#11668=CARTESIAN_POINT('',(-10.019478314682,97.837112635988,65.5));
#11669=CARTESIAN_POINT('',(-10.019478314682,97.837112635988,61.5));
#11670=CARTESIAN_POINT('',(-10.019478314682,97.837112635988,65.5));
#11671=CARTESIAN_POINT('',(-5.59729750026353,122.916546291862,65.5));
#11672=CARTESIAN_POINT('Origin',(4.79810263127257E-15,109.,65.5));
#11673=CARTESIAN_POINT('',(-5.59729750026353,122.916546291862,61.5));
#11674=CARTESIAN_POINT('',(-5.59729750026353,122.916546291862,65.5));
#11675=CARTESIAN_POINT('Origin',(4.79810263127257E-15,109.,61.5));
#11676=CARTESIAN_POINT('Origin',(4.79810263127257E-15,109.,65.5));
#11677=CARTESIAN_POINT('',(-9.25343387156297,97.1943250263015,61.5));
#11678=CARTESIAN_POINT('',(-9.25343387156298,97.1943250263015,65.5));
#11679=CARTESIAN_POINT('',(-9.25343387156297,97.1943250263015,65.5));
#11680=CARTESIAN_POINT('',(14.6770831941597,105.904320928824,61.5));
#11681=CARTESIAN_POINT('Origin',(4.79810263127257E-15,109.,61.5));
#11682=CARTESIAN_POINT('',(14.6770831941597,105.904320928824,65.5));
#11683=CARTESIAN_POINT('',(14.6770831941597,105.904320928824,65.5));
#11684=CARTESIAN_POINT('Origin',(4.79810263127257E-15,109.,65.5));
#11685=CARTESIAN_POINT('Origin',(4.79810263127257E-15,109.,65.5));
#11686=CARTESIAN_POINT('',(14.8507313718266,106.889128681836,61.5));
#11687=CARTESIAN_POINT('',(14.8507313718266,106.889128681836,65.5));
#11688=CARTESIAN_POINT('',(14.8507313718266,106.889128681836,65.5));
#11689=CARTESIAN_POINT('',(-4.65760487947762,123.258566435188,61.5));
#11690=CARTESIAN_POINT('Origin',(4.79810263127257E-15,109.,61.5));
#11691=CARTESIAN_POINT('',(-4.65760487947762,123.258566435188,65.5));
#11692=CARTESIAN_POINT('',(-4.65760487947762,123.258566435188,65.5));
#11693=CARTESIAN_POINT('Origin',(4.79810263127257E-15,109.,65.5));
#11694=CARTESIAN_POINT('Origin',(4.79810263127257E-15,109.,65.5));
#11695=CARTESIAN_POINT('',(-9.35047446273056,98.6344003800105,65.5));
#11696=CARTESIAN_POINT('',(-10.019478314682,97.837112635988,65.5));
#11697=CARTESIAN_POINT('',(-8.58443001961159,97.9916127703239,65.5));
#11698=CARTESIAN_POINT('',(-8.58443001961159,97.9916127703239,65.5));
#11699=CARTESIAN_POINT('',(-8.5844300196116,97.9916127703239,65.5));
#11700=CARTESIAN_POINT('',(13.6521098277345,106.085051387833,65.5));
#11701=CARTESIAN_POINT('',(14.6770831941597,105.904320928824,65.5));
#11702=CARTESIAN_POINT('',(13.8257580054015,107.069859140845,65.5));
#11703=CARTESIAN_POINT('',(13.8257580054015,107.069859140845,65.5));
#11704=CARTESIAN_POINT('',(13.8257580054015,107.069859140845,65.5));
#11705=CARTESIAN_POINT('',(-4.30163536500389,122.280548232157,65.5));
#11706=CARTESIAN_POINT('',(-4.65760487947762,123.258566435188,65.5));
#11707=CARTESIAN_POINT('',(-5.2413279857898,121.938528088831,65.5));
#11708=CARTESIAN_POINT('',(-5.2413279857898,121.938528088831,65.5));
#11709=CARTESIAN_POINT('',(-5.24132798578981,121.938528088831,65.5));
#11710=CARTESIAN_POINT('',(-13.,109.,65.5));
#11711=CARTESIAN_POINT('Origin',(4.79810263127257E-15,109.,65.5));
#11712=CARTESIAN_POINT('Origin',(0.,126.,-11.9999999999999));
#11713=CARTESIAN_POINT('',(0.,89.,16.16342581706));
#11714=CARTESIAN_POINT('Origin',(0.,89.,-11.9999999999999));
#11715=CARTESIAN_POINT('',(-1.72451246399432E-15,94.,16.16342581706));
#11716=CARTESIAN_POINT('',(-3.44902492798863E-15,126.,16.16342581706));
#11717=CARTESIAN_POINT('',(-15.,109.,11.8364962558057));
#11718=CARTESIAN_POINT('Ctrl Pts',(-15.,109.,11.8364962558057));
#11719=CARTESIAN_POINT('Ctrl Pts',(-15.,108.034202794276,11.8364962558057));
#11720=CARTESIAN_POINT('Ctrl Pts',(-14.9052762534063,107.044006310494,11.8969354528545));
#11721=CARTESIAN_POINT('Ctrl Pts',(-14.5155028930965,105.089329014181,12.1356781489979));
#11722=CARTESIAN_POINT('Ctrl Pts',(-14.2206269533151,104.124758926468,12.3135340099836));
#11723=CARTESIAN_POINT('Ctrl Pts',(-13.0649879364951,101.365664401063,12.9653152261472));
#11724=CARTESIAN_POINT('Ctrl Pts',(-11.9192829736626,99.7060795380662,13.5561572236054));
#11725=CARTESIAN_POINT('Ctrl Pts',(-9.29871093997433,97.0855075043779,14.6215293486697));
#11726=CARTESIAN_POINT('Ctrl Pts',(-7.63759490096063,95.9363382053097,15.1733726751026));
#11727=CARTESIAN_POINT('Ctrl Pts',(-4.8732166939491,94.7785446488243,15.7545840354958));
#11728=CARTESIAN_POINT('Ctrl Pts',(-3.9068153878956,94.4834357307163,15.9084529938547));
#11729=CARTESIAN_POINT('Ctrl Pts',(-1.95136354983184,94.0940942925199,16.1129353729621));
#11730=CARTESIAN_POINT('Ctrl Pts',(-0.962272640803981,94.,16.16342581706));
#11731=CARTESIAN_POINT('Ctrl Pts',(3.88578058618805E-15,94.,16.16342581706));
#11732=CARTESIAN_POINT('',(4.95933585255997E-16,124.,16.16342581706));
#11733=CARTESIAN_POINT('Ctrl Pts',(5.55111512312578E-15,124.,16.16342581706));
#11734=CARTESIAN_POINT('Ctrl Pts',(-0.962272640803984,124.,16.16342581706));
#11735=CARTESIAN_POINT('Ctrl Pts',(-1.95136354983183,123.90590570748,16.1129353729621));
#11736=CARTESIAN_POINT('Ctrl Pts',(-3.9068153878956,123.516564269284,15.9084529938547));
#11737=CARTESIAN_POINT('Ctrl Pts',(-4.87321669394909,123.221455351176,15.7545840354958));
#11738=CARTESIAN_POINT('Ctrl Pts',(-7.63759490096062,122.06366179469,15.1733726751026));
#11739=CARTESIAN_POINT('Ctrl Pts',(-9.29871093997433,120.914492495622,14.6215293486697));
#11740=CARTESIAN_POINT('Ctrl Pts',(-11.9192829736626,118.293920461934,13.5561572236054));
#11741=CARTESIAN_POINT('Ctrl Pts',(-13.0649879364951,116.634335598937,12.9653152261472));
#11742=CARTESIAN_POINT('Ctrl Pts',(-14.2206269533151,113.875241073532,12.3135340099836));
#11743=CARTESIAN_POINT('Ctrl Pts',(-14.5155028930965,112.910670985819,12.1356781489979));
#11744=CARTESIAN_POINT('Ctrl Pts',(-14.9052762534063,110.955993689506,11.8969354528545));
#11745=CARTESIAN_POINT('Ctrl Pts',(-15.,109.965797205724,11.8364962558057));
#11746=CARTESIAN_POINT('Ctrl Pts',(-15.,109.,11.8364962558057));
#11747=CARTESIAN_POINT('',(0.,126.,16.16342581706));
#11748=CARTESIAN_POINT('',(-3.44902492798863E-15,126.,16.16342581706));
#11749=CARTESIAN_POINT('Origin',(0.,126.,-11.9999999999999));
#11750=CARTESIAN_POINT('',(15.,109.,11.8364962558057));
#11751=CARTESIAN_POINT('Ctrl Pts',(15.,109.,11.8364962558057));
#11752=CARTESIAN_POINT('Ctrl Pts',(15.,109.965797205724,11.8364962558057));
#11753=CARTESIAN_POINT('Ctrl Pts',(14.9052762534063,110.955993689506,11.8969354528545));
#11754=CARTESIAN_POINT('Ctrl Pts',(14.5155028930965,112.910670985819,12.1356781489979));
#11755=CARTESIAN_POINT('Ctrl Pts',(14.2206269533151,113.875241073532,12.3135340099836));
#11756=CARTESIAN_POINT('Ctrl Pts',(13.0649879364951,116.634335598937,12.9653152261472));
#11757=CARTESIAN_POINT('Ctrl Pts',(11.9192829736626,118.293920461934,13.5561572236054));
#11758=CARTESIAN_POINT('Ctrl Pts',(9.29871093997435,120.914492495622,14.6215293486697));
#11759=CARTESIAN_POINT('Ctrl Pts',(7.63759490096064,122.06366179469,15.1733726751026));
#11760=CARTESIAN_POINT('Ctrl Pts',(4.87321669394911,123.221455351176,15.7545840354958));
#11761=CARTESIAN_POINT('Ctrl Pts',(3.90681538789561,123.516564269284,15.9084529938547));
#11762=CARTESIAN_POINT('Ctrl Pts',(1.95136354983185,123.90590570748,16.1129353729621));
#11763=CARTESIAN_POINT('Ctrl Pts',(0.962272640803995,124.,16.16342581706));
#11764=CARTESIAN_POINT('Ctrl Pts',(5.82867087928207E-15,124.,16.16342581706));
#11765=CARTESIAN_POINT('Ctrl Pts',(2.22044604925031E-15,94.,16.16342581706));
#11766=CARTESIAN_POINT('Ctrl Pts',(0.962272640803993,94.,16.16342581706));
#11767=CARTESIAN_POINT('Ctrl Pts',(1.95136354983185,94.0940942925199,16.1129353729621));
#11768=CARTESIAN_POINT('Ctrl Pts',(3.90681538789561,94.4834357307163,15.9084529938547));
#11769=CARTESIAN_POINT('Ctrl Pts',(4.87321669394911,94.7785446488243,15.7545840354958));
#11770=CARTESIAN_POINT('Ctrl Pts',(7.63759490096064,95.9363382053097,15.1733726751026));
#11771=CARTESIAN_POINT('Ctrl Pts',(9.29871093997435,97.0855075043779,14.6215293486697));
#11772=CARTESIAN_POINT('Ctrl Pts',(11.9192829736626,99.7060795380662,13.5561572236054));
#11773=CARTESIAN_POINT('Ctrl Pts',(13.0649879364951,101.365664401063,12.9653152261472));
#11774=CARTESIAN_POINT('Ctrl Pts',(14.2206269533151,104.124758926468,12.3135340099836));
#11775=CARTESIAN_POINT('Ctrl Pts',(14.5155028930965,105.089329014181,12.1356781489979));
#11776=CARTESIAN_POINT('Ctrl Pts',(14.9052762534063,107.044006310494,11.8969354528545));
#11777=CARTESIAN_POINT('Ctrl Pts',(15.,108.034202794276,11.8364962558057));
#11778=CARTESIAN_POINT('Ctrl Pts',(15.,109.,11.8364962558057));
#11779=CARTESIAN_POINT('',(-28.1430112947403,109.,-10.9278670711363));
#11780=CARTESIAN_POINT('',(-13.1430112947402,109.,-36.9086291846694));
#11781=CARTESIAN_POINT('Ctrl Pts',(-28.1430112947403,109.,-10.9278670711363));
#11782=CARTESIAN_POINT('Ctrl Pts',(-28.1430112947403,109.965797205724,-10.9278670711363));
#11783=CARTESIAN_POINT('Ctrl Pts',(-28.1479913014721,110.955993689506,-11.0401198405525));
#11784=CARTESIAN_POINT('Ctrl Pts',(-28.1598618611454,112.910670985819,-11.4970448203709));
#11785=CARTESIAN_POINT('Ctrl Pts',(-28.1664515850802,113.875241073532,-11.8413428056792));
#11786=CARTESIAN_POINT('Ctrl Pts',(-28.1530911675774,116.634335598937,-13.1680461599316));
#11787=CARTESIAN_POINT('Ctrl Pts',(-28.0919228655826,118.293920461934,-14.4556767617156));
#11788=CARTESIAN_POINT('Ctrl Pts',(-27.7042761735281,120.914492495622,-17.2578447778688));
#11789=CARTESIAN_POINT('Ctrl Pts',(-27.351628493621,122.06366179469,-18.9723351295049));
#11790=CARTESIAN_POINT('Ctrl Pts',(-26.4727831931838,123.221455351176,-21.6569625626416));
#11791=CARTESIAN_POINT('Ctrl Pts',(-26.1228369669497,123.516564269284,-22.5708251231138));
#11792=CARTESIAN_POINT('Ctrl Pts',(-25.3221979828512,123.90590570748,-24.3665372803077));
#11793=CARTESIAN_POINT('Ctrl Pts',(-24.8713785355743,124.,-25.248360356227));
#11794=CARTESIAN_POINT('Ctrl Pts',(-23.9091058947703,124.,-26.915065460833));
#11795=CARTESIAN_POINT('Ctrl Pts',(-23.3708344330193,123.90590570748,-27.7463980926544));
#11796=CARTESIAN_POINT('Ctrl Pts',(-22.2160215790541,123.516564269284,-29.3376278707409));
#11797=CARTESIAN_POINT('Ctrl Pts',(-21.5995664992347,123.221455351176,-30.0976214728542));
#11798=CARTESIAN_POINT('Ctrl Pts',(-19.7140335926603,122.06366179469,-32.2010375455977));
#11799=CARTESIAN_POINT('Ctrl Pts',(-18.4055652335537,120.914492495622,-33.3636845708009));
#11800=CARTESIAN_POINT('Ctrl Pts',(-16.17263989192,118.293920461934,-35.1004804618898));
#11801=CARTESIAN_POINT('Ctrl Pts',(-15.0881032310822,116.634335598937,-35.7972690662155));
#11802=CARTESIAN_POINT('Ctrl Pts',(-13.9458246317649,113.875241073532,-36.4721912043043));
#11803=CARTESIAN_POINT('Ctrl Pts',(-13.6443589680487,112.910670985819,-36.638633328627));
#11804=CARTESIAN_POINT('Ctrl Pts',(-13.2427150480657,110.955993689506,-36.856815612302));
#11805=CARTESIAN_POINT('Ctrl Pts',(-13.1430112947402,109.965797205724,-36.9086291846694));
#11806=CARTESIAN_POINT('Ctrl Pts',(-13.1430112947402,109.,-36.9086291846694));
#11807=CARTESIAN_POINT('Ctrl Pts',(-13.1430112947402,109.,-36.9086291846694));
#11808=CARTESIAN_POINT('Ctrl Pts',(-13.1430112947402,108.034202794276,-36.9086291846694));
#11809=CARTESIAN_POINT('Ctrl Pts',(-13.2427150480657,107.044006310494,-36.856815612302));
#11810=CARTESIAN_POINT('Ctrl Pts',(-13.6443589680487,105.089329014181,-36.638633328627));
#11811=CARTESIAN_POINT('Ctrl Pts',(-13.9458246317649,104.124758926468,-36.4721912043043));
#11812=CARTESIAN_POINT('Ctrl Pts',(-15.0881032310822,101.365664401063,-35.7972690662155));
#11813=CARTESIAN_POINT('Ctrl Pts',(-16.17263989192,99.7060795380662,-35.1004804618898));
#11814=CARTESIAN_POINT('Ctrl Pts',(-18.4055652335537,97.0855075043779,-33.3636845708009));
#11815=CARTESIAN_POINT('Ctrl Pts',(-19.7140335926603,95.9363382053097,-32.2010375455977));
#11816=CARTESIAN_POINT('Ctrl Pts',(-21.5995664992347,94.7785446488243,-30.0976214728542));
#11817=CARTESIAN_POINT('Ctrl Pts',(-22.2160215790541,94.4834357307163,-29.3376278707409));
#11818=CARTESIAN_POINT('Ctrl Pts',(-23.3708344330193,94.0940942925199,-27.7463980926544));
#11819=CARTESIAN_POINT('Ctrl Pts',(-23.9091058947703,94.,-26.915065460833));
#11820=CARTESIAN_POINT('Ctrl Pts',(-24.8713785355743,94.,-25.248360356227));
#11821=CARTESIAN_POINT('Ctrl Pts',(-25.3221979828512,94.0940942925199,-24.3665372803077));
#11822=CARTESIAN_POINT('Ctrl Pts',(-26.1228369669498,94.4834357307163,-22.5708251231138));
#11823=CARTESIAN_POINT('Ctrl Pts',(-26.4727831931838,94.7785446488243,-21.6569625626416));
#11824=CARTESIAN_POINT('Ctrl Pts',(-27.351628493621,95.9363382053097,-18.9723351295049));
#11825=CARTESIAN_POINT('Ctrl Pts',(-27.7042761735281,97.0855075043779,-17.2578447778688));
#11826=CARTESIAN_POINT('Ctrl Pts',(-28.0919228655826,99.7060795380662,-14.4556767617156));
#11827=CARTESIAN_POINT('Ctrl Pts',(-28.1530911675774,101.365664401063,-13.1680461599316));
#11828=CARTESIAN_POINT('Ctrl Pts',(-28.1664515850802,104.124758926468,-11.8413428056792));
#11829=CARTESIAN_POINT('Ctrl Pts',(-28.1598618611454,105.089329014181,-11.4970448203709));
#11830=CARTESIAN_POINT('Ctrl Pts',(-28.1479913014721,107.044006310494,-11.0401198405525));
#11831=CARTESIAN_POINT('Ctrl Pts',(-28.1430112947403,108.034202794276,-10.9278670711363));
#11832=CARTESIAN_POINT('Ctrl Pts',(-28.1430112947403,109.,-10.9278670711363));
#11833=CARTESIAN_POINT('',(13.1430112947406,109.,-36.9086291846692));
#11834=CARTESIAN_POINT('',(28.1430112947403,109.,-10.9278670711359));
#11835=CARTESIAN_POINT('Ctrl Pts',(13.1430112947406,109.,-36.9086291846692));
#11836=CARTESIAN_POINT('Ctrl Pts',(13.1430112947406,109.965797205724,-36.9086291846692));
#11837=CARTESIAN_POINT('Ctrl Pts',(13.2427150480661,110.955993689506,-36.8568156123018));
#11838=CARTESIAN_POINT('Ctrl Pts',(13.6443589680491,112.910670985819,-36.6386333286268));
#11839=CARTESIAN_POINT('Ctrl Pts',(13.9458246317653,113.875241073532,-36.4721912043041));
#11840=CARTESIAN_POINT('Ctrl Pts',(15.0881032310825,116.634335598937,-35.7972690662153));
#11841=CARTESIAN_POINT('Ctrl Pts',(16.1726398919203,118.293920461934,-35.1004804618895));
#11842=CARTESIAN_POINT('Ctrl Pts',(18.4055652335539,120.914492495622,-33.3636845708006));
#11843=CARTESIAN_POINT('Ctrl Pts',(19.7140335926606,122.06366179469,-32.2010375455974));
#11844=CARTESIAN_POINT('Ctrl Pts',(21.5995664992349,123.221455351176,-30.0976214728539));
#11845=CARTESIAN_POINT('Ctrl Pts',(22.2160215790544,123.516564269284,-29.3376278707406));
#11846=CARTESIAN_POINT('Ctrl Pts',(23.3708344330195,123.90590570748,-27.7463980926541));
#11847=CARTESIAN_POINT('Ctrl Pts',(23.9091058947705,124.,-26.9150654608326));
#11848=CARTESIAN_POINT('Ctrl Pts',(24.8713785355745,124.,-25.2483603562266));
#11849=CARTESIAN_POINT('Ctrl Pts',(25.3221979828513,123.90590570748,-24.3665372803074));
#11850=CARTESIAN_POINT('Ctrl Pts',(26.1228369669499,123.516564269284,-22.5708251231135));
#11851=CARTESIAN_POINT('Ctrl Pts',(26.4727831931839,123.221455351176,-21.6569625626412));
#11852=CARTESIAN_POINT('Ctrl Pts',(27.3516284936211,122.06366179469,-18.9723351295045));
#11853=CARTESIAN_POINT('Ctrl Pts',(27.7042761735281,120.914492495622,-17.2578447778684));
#11854=CARTESIAN_POINT('Ctrl Pts',(28.0919228655827,118.293920461934,-14.4556767617152));
#11855=CARTESIAN_POINT('Ctrl Pts',(28.1530911675774,116.634335598937,-13.1680461599312));
#11856=CARTESIAN_POINT('Ctrl Pts',(28.1664515850802,113.875241073532,-11.8413428056788));
#11857=CARTESIAN_POINT('Ctrl Pts',(28.1598618611454,112.910670985819,-11.4970448203705));
#11858=CARTESIAN_POINT('Ctrl Pts',(28.1479913014721,110.955993689506,-11.0401198405521));
#11859=CARTESIAN_POINT('Ctrl Pts',(28.1430112947403,109.965797205724,-10.9278670711359));
#11860=CARTESIAN_POINT('Ctrl Pts',(28.1430112947403,109.,-10.9278670711359));
#11861=CARTESIAN_POINT('Ctrl Pts',(28.1430112947403,109.,-10.9278670711359));
#11862=CARTESIAN_POINT('Ctrl Pts',(28.1430112947403,108.034202794276,-10.9278670711359));
#11863=CARTESIAN_POINT('Ctrl Pts',(28.1479913014721,107.044006310494,-11.0401198405521));
#11864=CARTESIAN_POINT('Ctrl Pts',(28.1598618611454,105.089329014181,-11.4970448203705));
#11865=CARTESIAN_POINT('Ctrl Pts',(28.1664515850802,104.124758926468,-11.8413428056788));
#11866=CARTESIAN_POINT('Ctrl Pts',(28.1530911675774,101.365664401063,-13.1680461599312));
#11867=CARTESIAN_POINT('Ctrl Pts',(28.0919228655827,99.7060795380662,-14.4556767617152));
#11868=CARTESIAN_POINT('Ctrl Pts',(27.7042761735281,97.0855075043779,-17.2578447778684));
#11869=CARTESIAN_POINT('Ctrl Pts',(27.3516284936211,95.9363382053097,-18.9723351295045));
#11870=CARTESIAN_POINT('Ctrl Pts',(26.4727831931839,94.7785446488243,-21.6569625626412));
#11871=CARTESIAN_POINT('Ctrl Pts',(26.1228369669499,94.4834357307163,-22.5708251231135));
#11872=CARTESIAN_POINT('Ctrl Pts',(25.3221979828513,94.0940942925199,-24.3665372803074));
#11873=CARTESIAN_POINT('Ctrl Pts',(24.8713785355745,94.,-25.2483603562266));
#11874=CARTESIAN_POINT('Ctrl Pts',(23.9091058947705,94.,-26.9150654608326));
#11875=CARTESIAN_POINT('Ctrl Pts',(23.3708344330195,94.0940942925199,-27.7463980926541));
#11876=CARTESIAN_POINT('Ctrl Pts',(22.2160215790544,94.4834357307163,-29.3376278707406));
#11877=CARTESIAN_POINT('Ctrl Pts',(21.5995664992349,94.7785446488243,-30.0976214728539));
#11878=CARTESIAN_POINT('Ctrl Pts',(19.7140335926605,95.9363382053097,-32.2010375455974));
#11879=CARTESIAN_POINT('Ctrl Pts',(18.4055652335539,97.0855075043779,-33.3636845708006));
#11880=CARTESIAN_POINT('Ctrl Pts',(16.1726398919203,99.7060795380662,-35.1004804618895));
#11881=CARTESIAN_POINT('Ctrl Pts',(15.0881032310825,101.365664401063,-35.7972690662153));
#11882=CARTESIAN_POINT('Ctrl Pts',(13.9458246317653,104.124758926468,-36.4721912043041));
#11883=CARTESIAN_POINT('Ctrl Pts',(13.6443589680491,105.089329014181,-36.6386333286268));
#11884=CARTESIAN_POINT('Ctrl Pts',(13.242715048066,107.044006310494,-36.8568156123018));
#11885=CARTESIAN_POINT('Ctrl Pts',(13.1430112947406,108.034202794276,-36.9086291846692));
#11886=CARTESIAN_POINT('Ctrl Pts',(13.1430112947406,109.,-36.9086291846692));
#11887=CARTESIAN_POINT('Origin',(0.,126.,-11.9999999999999));
#11888=CARTESIAN_POINT('',(-2.83670152841496E-15,126.,-35.1634258170598));
#11889=CARTESIAN_POINT('Origin',(0.,126.,-11.9999999999999));
#11890=CARTESIAN_POINT('Origin',(0.,89.,-11.9999999999999));
#11891=CARTESIAN_POINT('',(-2.44929359829471E-15,89.,8.00000000000008));
#11892=CARTESIAN_POINT('Origin',(0.,89.,-11.9999999999999));
#11893=CARTESIAN_POINT('Origin',(0.,125.,-11.9999999999999));
#11894=CARTESIAN_POINT('',(-2.83670152841496E-15,125.,-35.1634258170598));
#11895=CARTESIAN_POINT('Origin',(0.,125.,-11.9999999999999));
#11896=CARTESIAN_POINT('',(-2.83670152841496E-15,125.,-35.1634258170598));
#11897=CARTESIAN_POINT('Origin',(0.,125.,-11.9999999999999));
#11898=CARTESIAN_POINT('Origin',(4.79810263127257E-15,109.,-191.42723747195));
#11899=CARTESIAN_POINT('',(-15.,109.,57.5));
#11900=CARTESIAN_POINT('Origin',(4.79810263127257E-15,109.,57.5));
#11901=CARTESIAN_POINT('',(-15.,109.,-191.42723747195));
#11902=CARTESIAN_POINT('Origin',(4.79810263127257E-15,109.,61.5));
#11903=CARTESIAN_POINT('',(17.,109.,61.5));
#11904=CARTESIAN_POINT('Origin',(4.79810263127257E-15,109.,61.5));
#11905=CARTESIAN_POINT('',(-8.58443001961159,97.9916127703239,61.5));
#11906=CARTESIAN_POINT('',(-8.58443001961159,97.9916127703239,61.5));
#11907=CARTESIAN_POINT('',(-9.35047446273056,98.6344003800105,61.5));
#11908=CARTESIAN_POINT('',(-8.58443001961159,97.9916127703239,61.5));
#11909=CARTESIAN_POINT('',(-9.35047446273056,98.6344003800105,61.5));
#11910=CARTESIAN_POINT('',(-5.2413279857898,121.938528088831,61.5));
#11911=CARTESIAN_POINT('',(-5.2413279857898,121.938528088831,61.5));
#11912=CARTESIAN_POINT('',(-4.30163536500389,122.280548232157,61.5));
#11913=CARTESIAN_POINT('',(-5.2413279857898,121.938528088831,61.5));
#11914=CARTESIAN_POINT('',(-4.30163536500389,122.280548232157,61.5));
#11915=CARTESIAN_POINT('',(13.8257580054015,107.069859140845,61.5));
#11916=CARTESIAN_POINT('',(13.8257580054015,107.069859140845,61.5));
#11917=CARTESIAN_POINT('',(13.6521098277345,106.085051387833,61.5));
#11918=CARTESIAN_POINT('',(13.8257580054015,107.069859140845,61.5));
#11919=CARTESIAN_POINT('',(13.6521098277345,106.085051387833,61.5));
#11920=CARTESIAN_POINT('Origin',(4.79810263127257E-15,109.,61.5));
#11921=CARTESIAN_POINT('',(17.,109.,59.5));
#11922=CARTESIAN_POINT('',(-17.,109.,59.5));
#11923=CARTESIAN_POINT('Origin',(4.79810263127257E-15,109.,59.5));
#11924=CARTESIAN_POINT('Origin',(4.79810263127257E-15,109.,59.5));
#11925=CARTESIAN_POINT('',(17.,109.,61.5));
#11926=CARTESIAN_POINT('Origin',(4.79810263127257E-15,109.,-191.42723747195));
#11927=CARTESIAN_POINT('',(12.999999999998,109.,3.19868415357247));
#11928=CARTESIAN_POINT('',(3.63257893358771E-15,122.,8.00000000000008));
#11929=CARTESIAN_POINT('Ctrl Pts',(13.,109.,3.19868415357074));
#11930=CARTESIAN_POINT('Ctrl Pts',(13.,109.851995783248,3.19868415357074));
#11931=CARTESIAN_POINT('Ctrl Pts',(12.9150719143893,110.718692707522,3.27253856324928));
#11932=CARTESIAN_POINT('Ctrl Pts',(12.5720677115743,112.41995630624,3.55611229413735));
#11933=CARTESIAN_POINT('Ctrl Pts',(12.3141919444307,113.25470217185,3.76499824413062));
#11934=CARTESIAN_POINT('Ctrl Pts',(11.3107639081373,115.63581455956,4.51558245123477));
#11935=CARTESIAN_POINT('Ctrl Pts',(10.3239083354049,117.060867975445,5.17673327565937));
#11936=CARTESIAN_POINT('Ctrl Pts',(8.07178308824895,119.312993222601,6.34225725186619));
#11937=CARTESIAN_POINT('Ctrl Pts',(6.64417608295783,120.307169987275,6.93603058768733));
#11938=CARTESIAN_POINT('Ctrl Pts',(4.25116977785989,121.315715660585,7.56034611361149));
#11939=CARTESIAN_POINT('Ctrl Pts',(3.41196563272457,121.574314859725,7.72552166608632));
#11940=CARTESIAN_POINT('Ctrl Pts',(1.70829130581225,121.916526022509,7.94541188586552));
#11941=CARTESIAN_POINT('Ctrl Pts',(0.843777078670328,122.,8.00000000000008));
#11942=CARTESIAN_POINT('Ctrl Pts',(9.15933995315754E-15,122.,8.00000000000008));
#11943=CARTESIAN_POINT('',(2.43541035559477E-17,96.,8.00000000000008));
#11944=CARTESIAN_POINT('Ctrl Pts',(1.94289029309402E-15,96.,8.00000000000008));
#11945=CARTESIAN_POINT('Ctrl Pts',(0.84377707867032,96.,8.00000000000008));
#11946=CARTESIAN_POINT('Ctrl Pts',(1.70829130581224,96.0834739774908,7.94541188586552));
#11947=CARTESIAN_POINT('Ctrl Pts',(3.41196563272457,96.4256851402753,7.72552166608632));
#11948=CARTESIAN_POINT('Ctrl Pts',(4.25116977785989,96.6842843394153,7.56034611361149));
#11949=CARTESIAN_POINT('Ctrl Pts',(6.64417608295782,97.692830012725,6.93603058768733));
#11950=CARTESIAN_POINT('Ctrl Pts',(8.07178308824894,98.6870067773987,6.3422572518662));
#11951=CARTESIAN_POINT('Ctrl Pts',(10.3239083354049,100.939132024555,5.17673327565937));
#11952=CARTESIAN_POINT('Ctrl Pts',(11.3107639081373,102.36418544044,4.51558245123478));
#11953=CARTESIAN_POINT('Ctrl Pts',(12.3141919444307,104.74529782815,3.76499824413063));
#11954=CARTESIAN_POINT('Ctrl Pts',(12.5720677115743,105.58004369376,3.55611229413735));
#11955=CARTESIAN_POINT('Ctrl Pts',(12.9150719143893,107.281307292478,3.27253856324928));
#11956=CARTESIAN_POINT('Ctrl Pts',(13.,108.148004216753,3.19868415357074));
#11957=CARTESIAN_POINT('Ctrl Pts',(13.,109.,3.19868415357074));
#11958=CARTESIAN_POINT('',(-13.,109.,3.19868415357075));
#11959=CARTESIAN_POINT('Ctrl Pts',(-13.,109.,3.19868415357075));
#11960=CARTESIAN_POINT('Ctrl Pts',(-13.,108.148004216753,3.19868415357075));
#11961=CARTESIAN_POINT('Ctrl Pts',(-12.9150719143893,107.281307292478,3.27253856324928));
#11962=CARTESIAN_POINT('Ctrl Pts',(-12.5720677115743,105.58004369376,3.55611229413736));
#11963=CARTESIAN_POINT('Ctrl Pts',(-12.3141919444307,104.74529782815,3.76499824413063));
#11964=CARTESIAN_POINT('Ctrl Pts',(-11.3107639081373,102.36418544044,4.51558245123478));
#11965=CARTESIAN_POINT('Ctrl Pts',(-10.3239083354049,100.939132024555,5.17673327565937));
#11966=CARTESIAN_POINT('Ctrl Pts',(-8.07178308824894,98.6870067773987,6.3422572518662));
#11967=CARTESIAN_POINT('Ctrl Pts',(-6.64417608295782,97.692830012725,6.93603058768733));
#11968=CARTESIAN_POINT('Ctrl Pts',(-4.25116977785988,96.6842843394153,7.5603461136115));
#11969=CARTESIAN_POINT('Ctrl Pts',(-3.41196563272456,96.4256851402753,7.72552166608632));
#11970=CARTESIAN_POINT('Ctrl Pts',(-1.70829130581224,96.0834739774908,7.94541188586552));
#11971=CARTESIAN_POINT('Ctrl Pts',(-0.843777078670316,96.,8.00000000000008));
#11972=CARTESIAN_POINT('Ctrl Pts',(2.4980018054066E-15,96.,8.00000000000008));
#11973=CARTESIAN_POINT('',(-13.,109.,-191.42723747195));
#11974=CARTESIAN_POINT('Ctrl Pts',(8.60422844084496E-15,122.,8.00000000000008));
#11975=CARTESIAN_POINT('Ctrl Pts',(-0.843777078670309,122.,8.00000000000008));
#11976=CARTESIAN_POINT('Ctrl Pts',(-1.70829130581223,121.916526022509,7.94541188586552));
#11977=CARTESIAN_POINT('Ctrl Pts',(-3.41196563272456,121.574314859725,7.72552166608632));
#11978=CARTESIAN_POINT('Ctrl Pts',(-4.25116977785987,121.315715660585,7.5603461136115));
#11979=CARTESIAN_POINT('Ctrl Pts',(-6.64417608295781,120.307169987275,6.93603058768734));
#11980=CARTESIAN_POINT('Ctrl Pts',(-8.07178308824893,119.312993222601,6.3422572518662));
#11981=CARTESIAN_POINT('Ctrl Pts',(-10.3239083354049,117.060867975445,5.17673327565938));
#11982=CARTESIAN_POINT('Ctrl Pts',(-11.3107639081373,115.63581455956,4.51558245123479));
#11983=CARTESIAN_POINT('Ctrl Pts',(-12.3141919444307,113.25470217185,3.76499824413064));
#11984=CARTESIAN_POINT('Ctrl Pts',(-12.5720677115743,112.41995630624,3.55611229413736));
#11985=CARTESIAN_POINT('Ctrl Pts',(-12.9150719143893,110.718692707522,3.27253856324929));
#11986=CARTESIAN_POINT('Ctrl Pts',(-13.,109.851995783248,3.19868415357075));
#11987=CARTESIAN_POINT('Ctrl Pts',(-13.,109.,3.19868415357075));
#11988=CARTESIAN_POINT('Origin',(4.79810263127257E-15,109.,59.5));
#11989=CARTESIAN_POINT('',(-17.,109.,59.5));
#11990=CARTESIAN_POINT('Origin',(-54.6822367721436,109.,19.5708041202874));
#11991=CARTESIAN_POINT('',(67.6887655630186,109.,-33.7596189432327));
#11992=CARTESIAN_POINT('Origin',(60.1887655630187,109.,-46.7499999999993));
#11993=CARTESIAN_POINT('',(-47.1822367721437,109.,32.561185177054));
#11994=CARTESIAN_POINT('Origin',(54.6822367721438,109.,19.5708041202885));
#11995=CARTESIAN_POINT('',(-52.6887655630182,109.,-59.7403810567667));
#11996=CARTESIAN_POINT('Origin',(-60.1887655630183,109.,-46.7500000000002));
#11997=CARTESIAN_POINT('',(62.1822367721439,109.,6.58042306352195));
#11998=CARTESIAN_POINT('Origin',(-63.6528671781565,109.,-48.7499999999993));
#11999=CARTESIAN_POINT('',(-72.1528671781564,109.,-34.0275681356638));
#12000=CARTESIAN_POINT('Origin',(-63.6528671781565,109.,-48.7499999999993));
#12001=CARTESIAN_POINT('',(-61.5020494956546,122.280548232157,-52.4753255039102));
#12002=CARTESIAN_POINT('',(-61.5020494956546,122.280548232157,-52.4753255039102));
#12003=CARTESIAN_POINT('',(-70.5657461808571,107.069859140845,-36.7765423407455));
#12004=CARTESIAN_POINT('',(-70.5657461808571,107.069859140845,-36.7765423407455));
#12005=CARTESIAN_POINT('',(-70.4789220920237,106.085051387833,-36.9269260739259));
#12006=CARTESIAN_POINT('',(-70.5657461808571,107.069859140845,-36.7765423407455));
#12007=CARTESIAN_POINT('',(-70.4789220920237,106.085051387833,-36.9269260739259));
#12008=CARTESIAN_POINT('',(-59.3606521683508,97.9916127703239,-56.1843344739927));
#12009=CARTESIAN_POINT('',(-59.3606521683508,97.9916127703239,-56.1843344739927));
#12010=CARTESIAN_POINT('',(-58.9776299467913,98.6344003800105,-56.8477484221616));
#12011=CARTESIAN_POINT('',(-59.3606521683508,97.9916127703239,-56.1843344739927));
#12012=CARTESIAN_POINT('',(-58.9776299467913,98.6344003800105,-56.8477484221616));
#12013=CARTESIAN_POINT('',(-61.0322031852617,121.938528088831,-53.2891231852596));
#12014=CARTESIAN_POINT('',(-61.0322031852617,121.938528088831,-53.2891231852596));
#12015=CARTESIAN_POINT('',(-61.0322031852617,121.938528088831,-53.2891231852596));
#12016=CARTESIAN_POINT('Origin',(-63.6528671781565,109.,-48.7499999999993));
#12017=CARTESIAN_POINT('',(-70.4208163705874,109.,-33.0275681356637));
#12018=CARTESIAN_POINT('',(-53.4208163705878,109.,-62.4724318643349));
#12019=CARTESIAN_POINT('Origin',(-61.9208163705876,109.,-47.7499999999993));
#12020=CARTESIAN_POINT('Origin',(-61.9208163705876,109.,-47.7499999999993));
#12021=CARTESIAN_POINT('',(-72.1528671781564,109.,-34.0275681356638));
#12022=CARTESIAN_POINT('Origin',(63.652867178156,109.,-48.7500000000002));
#12023=CARTESIAN_POINT('',(55.152867178156,109.,-63.4724318643356));
#12024=CARTESIAN_POINT('Origin',(63.652867178156,109.,-48.7500000000002));
#12025=CARTESIAN_POINT('',(65.803684860658,122.280548232157,-45.0246744960893));
#12026=CARTESIAN_POINT('',(65.803684860658,122.280548232157,-45.0246744960893));
#12027=CARTESIAN_POINT('',(56.7399881754552,107.069859140845,-60.7234576592539));
#12028=CARTESIAN_POINT('',(56.7399881754552,107.069859140845,-60.7234576592539));
#12029=CARTESIAN_POINT('',(56.8268122642887,106.085051387833,-60.5730739260735));
#12030=CARTESIAN_POINT('',(56.7399881754552,107.069859140845,-60.7234576592539));
#12031=CARTESIAN_POINT('',(56.8268122642887,106.085051387833,-60.5730739260735));
#12032=CARTESIAN_POINT('',(67.9450821879618,97.991612770324,-41.3156655260068));
#12033=CARTESIAN_POINT('',(67.9450821879618,97.991612770324,-41.3156655260068));
#12034=CARTESIAN_POINT('',(68.3281044095213,98.6344003800105,-40.6522515778379));
#12035=CARTESIAN_POINT('',(67.9450821879618,97.991612770324,-41.3156655260068));
#12036=CARTESIAN_POINT('',(68.3281044095213,98.6344003800105,-40.6522515778379));
#12037=CARTESIAN_POINT('',(66.2735311710509,121.938528088831,-44.2108768147399));
#12038=CARTESIAN_POINT('',(66.2735311710509,121.938528088831,-44.2108768147399));
#12039=CARTESIAN_POINT('',(66.2735311710509,121.938528088831,-44.2108768147399));
#12040=CARTESIAN_POINT('Origin',(63.652867178156,109.,-48.7500000000002));
#12041=CARTESIAN_POINT('',(53.4208163705871,109.,-62.4724318643356));
#12042=CARTESIAN_POINT('',(70.4208163705872,109.,-33.0275681356648));
#12043=CARTESIAN_POINT('Origin',(61.9208163705871,109.,-47.7500000000002));
#12044=CARTESIAN_POINT('Origin',(61.9208163705871,109.,-47.7500000000002));
#12045=CARTESIAN_POINT('',(55.152867178156,109.,-63.4724318643356));
#12046=CARTESIAN_POINT('Origin',(84.3262415816127,109.,36.6857782768941));
#12047=CARTESIAN_POINT('',(-19.6624465810882,109.,-8.34101182758738));
#12048=CARTESIAN_POINT('',(-6.66244658108813,109.,-30.857672325983));
#12049=CARTESIAN_POINT('Ctrl Pts',(-19.6624465810882,109.,-8.34101182758764));
#12050=CARTESIAN_POINT('Ctrl Pts',(-19.6624465810882,109.851995783248,-8.34101182758764));
#12051=CARTESIAN_POINT('Ctrl Pts',(-19.683942333246,110.718692707522,-8.45148891206053));
#12052=CARTESIAN_POINT('Ctrl Pts',(-19.7580222866335,112.41995630624,-8.89032613074718));
#12053=CARTESIAN_POINT('Ctrl Pts',(-19.8099849422495,113.25470217185,-9.21809607111061));
#12054=CARTESIAN_POINT('Ctrl Pts',(-19.9582959151344,115.63581455956,-10.4623823449623));
#12055=CARTESIAN_POINT('Ctrl Pts',(-20.0374415384529,117.060867975445,-11.6475997530271));
#12056=CARTESIAN_POINT('Ctrl Pts',(-19.9207522869899,119.312993222601,-14.1807594176719));
#12057=CARTESIAN_POINT('Ctrl Pts',(-19.7211715772552,120.307169987275,-15.7139900187852));
#12058=CARTESIAN_POINT('Ctrl Pts',(-19.0653415301336,121.315715660585,-18.0985520333784));
#12059=CARTESIAN_POINT('Ctrl Pts',(-18.7887856820933,121.574314859725,-18.9079119182642));
#12060=CARTESIAN_POINT('Ctrl Pts',(-18.1273790350096,121.916526022509,-20.4932822750352));
#12061=CARTESIAN_POINT('Ctrl Pts',(-17.7423966150239,122.,-21.2692676147405));
#12062=CARTESIAN_POINT('Ctrl Pts',(-16.8986195363536,122.,-22.7307323852595));
#12063=CARTESIAN_POINT('Ctrl Pts',(-16.4190877291974,121.916526022509,-23.4521296108302));
#12064=CARTESIAN_POINT('Ctrl Pts',(-15.3768200493687,121.574314859725,-24.817609747822));
#12065=CARTESIAN_POINT('Ctrl Pts',(-14.8141717522737,121.315715660585,-25.461794080233));
#12066=CARTESIAN_POINT('Ctrl Pts',(-13.0769954942974,120.307169987275,-27.2220405689021));
#12067=CARTESIAN_POINT('Ctrl Pts',(-11.8489691987409,119.312993222601,-28.1614978341942));
#12068=CARTESIAN_POINT('Ctrl Pts',(-9.71353320304791,117.060867975445,-29.5291335226322));
#12069=CARTESIAN_POINT('Ctrl Pts',(-8.647532006997,115.63581455956,-30.0532001062724));
#12070=CARTESIAN_POINT('Ctrl Pts',(-7.49579299781871,113.25470217185,-30.5469021730199));
#12071=CARTESIAN_POINT('Ctrl Pts',(-7.18595457505908,112.41995630624,-30.66578616339));
#12072=CARTESIAN_POINT('Ctrl Pts',(-6.76887041885657,110.718692707522,-30.8210496511886));
#12073=CARTESIAN_POINT('Ctrl Pts',(-6.6624465810881,109.851995783248,-30.857672325983));
#12074=CARTESIAN_POINT('Ctrl Pts',(-6.6624465810881,109.,-30.857672325983));
#12075=CARTESIAN_POINT('Ctrl Pts',(-6.6624465810881,109.,-30.857672325983));
#12076=CARTESIAN_POINT('Ctrl Pts',(-6.6624465810881,108.148004216753,-30.857672325983));
#12077=CARTESIAN_POINT('Ctrl Pts',(-6.76887041885657,107.281307292478,-30.8210496511886));
#12078=CARTESIAN_POINT('Ctrl Pts',(-7.18595457505907,105.58004369376,-30.66578616339));
#12079=CARTESIAN_POINT('Ctrl Pts',(-7.4957929978187,104.74529782815,-30.5469021730199));
#12080=CARTESIAN_POINT('Ctrl Pts',(-8.64753200699699,102.36418544044,-30.0532001062724));
#12081=CARTESIAN_POINT('Ctrl Pts',(-9.7135332030479,100.939132024555,-29.5291335226322));
#12082=CARTESIAN_POINT('Ctrl Pts',(-11.8489691987408,98.6870067773987,-28.1614978341942));
#12083=CARTESIAN_POINT('Ctrl Pts',(-13.0769954942973,97.692830012725,-27.2220405689021));
#12084=CARTESIAN_POINT('Ctrl Pts',(-14.8141717522737,96.6842843394153,-25.461794080233));
#12085=CARTESIAN_POINT('Ctrl Pts',(-15.3768200493687,96.4256851402753,-24.817609747822));
#12086=CARTESIAN_POINT('Ctrl Pts',(-16.4190877291974,96.0834739774908,-23.4521296108302));
#12087=CARTESIAN_POINT('Ctrl Pts',(-16.8986195363536,96.,-22.7307323852595));
#12088=CARTESIAN_POINT('Ctrl Pts',(-17.7423966150239,96.,-21.2692676147405));
#12089=CARTESIAN_POINT('Ctrl Pts',(-18.1273790350096,96.0834739774909,-20.4932822750352));
#12090=CARTESIAN_POINT('Ctrl Pts',(-18.7887856820933,96.4256851402753,-18.9079119182642));
#12091=CARTESIAN_POINT('Ctrl Pts',(-19.0653415301336,96.6842843394153,-18.0985520333784));
#12092=CARTESIAN_POINT('Ctrl Pts',(-19.7211715772552,97.692830012725,-15.7139900187852));
#12093=CARTESIAN_POINT('Ctrl Pts',(-19.9207522869899,98.6870067773987,-14.1807594176719));
#12094=CARTESIAN_POINT('Ctrl Pts',(-20.0374415384529,100.939132024555,-11.6475997530271));
#12095=CARTESIAN_POINT('Ctrl Pts',(-19.9582959151344,102.36418544044,-10.4623823449623));
#12096=CARTESIAN_POINT('Ctrl Pts',(-19.8099849422495,104.74529782815,-9.21809607111062));
#12097=CARTESIAN_POINT('Ctrl Pts',(-19.7580222866335,105.58004369376,-8.8903261307472));
#12098=CARTESIAN_POINT('Ctrl Pts',(-19.683942333246,107.281307292478,-8.45148891206054));
#12099=CARTESIAN_POINT('Ctrl Pts',(-19.6624465810882,108.148004216753,-8.34101182758764));
#12100=CARTESIAN_POINT('Ctrl Pts',(-19.6624465810882,109.,-8.34101182758764));
#12101=CARTESIAN_POINT('',(90.8262415816127,109.,25.4274480276964));
#12102=CARTESIAN_POINT('Origin',(-84.3262415816127,109.,36.6857782768926));
#12103=CARTESIAN_POINT('',(6.66244658108983,109.,-30.8576723259824));
#12104=CARTESIAN_POINT('',(19.6624465810882,109.,-8.34101182758737));
#12105=CARTESIAN_POINT('Ctrl Pts',(6.66244658108836,109.,-30.8576723259829));
#12106=CARTESIAN_POINT('Ctrl Pts',(6.66244658108836,109.851995783247,-30.8576723259829));
#12107=CARTESIAN_POINT('Ctrl Pts',(6.76887041885683,110.718692707522,-30.8210496511885));
#12108=CARTESIAN_POINT('Ctrl Pts',(7.18595457505932,112.41995630624,-30.6657861633899));
#12109=CARTESIAN_POINT('Ctrl Pts',(7.49579299781897,113.25470217185,-30.5469021730198));
#12110=CARTESIAN_POINT('Ctrl Pts',(8.64753200699724,115.63581455956,-30.0532001062722));
#12111=CARTESIAN_POINT('Ctrl Pts',(9.71353320304815,117.060867975445,-29.5291335226321));
#12112=CARTESIAN_POINT('Ctrl Pts',(11.8489691987411,119.312993222601,-28.1614978341941));
#12113=CARTESIAN_POINT('Ctrl Pts',(13.0769954942976,120.307169987275,-27.2220405689019));
#12114=CARTESIAN_POINT('Ctrl Pts',(14.8141717522739,121.315715660585,-25.4617940802328));
#12115=CARTESIAN_POINT('Ctrl Pts',(15.3768200493689,121.574314859725,-24.8176097478218));
#12116=CARTESIAN_POINT('Ctrl Pts',(16.4190877291975,121.916526022509,-23.45212961083));
#12117=CARTESIAN_POINT('Ctrl Pts',(16.8986195363537,122.,-22.7307323852593));
#12118=CARTESIAN_POINT('Ctrl Pts',(17.742396615024,122.,-21.2692676147402));
#12119=CARTESIAN_POINT('Ctrl Pts',(18.1273790350098,121.916526022509,-20.493282275035));
#12120=CARTESIAN_POINT('Ctrl Pts',(18.7887856820934,121.574314859725,-18.9079119182639));
#12121=CARTESIAN_POINT('Ctrl Pts',(19.0653415301337,121.315715660585,-18.0985520333781));
#12122=CARTESIAN_POINT('Ctrl Pts',(19.7211715772553,120.307169987275,-15.7139900187849));
#12123=CARTESIAN_POINT('Ctrl Pts',(19.9207522869899,119.312993222601,-14.1807594176716));
#12124=CARTESIAN_POINT('Ctrl Pts',(20.0374415384529,117.060867975445,-11.6475997530268));
#12125=CARTESIAN_POINT('Ctrl Pts',(19.9582959151344,115.63581455956,-10.462382344962));
#12126=CARTESIAN_POINT('Ctrl Pts',(19.8099849422494,113.25470217185,-9.21809607111035));
#12127=CARTESIAN_POINT('Ctrl Pts',(19.7580222866334,112.41995630624,-8.89032613074693));
#12128=CARTESIAN_POINT('Ctrl Pts',(19.6839423332459,110.718692707522,-8.45148891206027));
#12129=CARTESIAN_POINT('Ctrl Pts',(19.6624465810881,109.851995783248,-8.34101182758737));
#12130=CARTESIAN_POINT('Ctrl Pts',(19.6624465810881,109.,-8.34101182758737));
#12131=CARTESIAN_POINT('Ctrl Pts',(19.6624465810881,109.,-8.34101182758737));
#12132=CARTESIAN_POINT('Ctrl Pts',(19.6624465810881,108.148004216753,-8.34101182758737));
#12133=CARTESIAN_POINT('Ctrl Pts',(19.6839423332459,107.281307292478,-8.45148891206027));
#12134=CARTESIAN_POINT('Ctrl Pts',(19.7580222866334,105.58004369376,-8.89032613074692));
#12135=CARTESIAN_POINT('Ctrl Pts',(19.8099849422494,104.74529782815,-9.21809607111035));
#12136=CARTESIAN_POINT('Ctrl Pts',(19.9582959151344,102.36418544044,-10.462382344962));
#12137=CARTESIAN_POINT('Ctrl Pts',(20.0374415384529,100.939132024555,-11.6475997530268));
#12138=CARTESIAN_POINT('Ctrl Pts',(19.9207522869899,98.6870067773987,-14.1807594176716));
#12139=CARTESIAN_POINT('Ctrl Pts',(19.7211715772553,97.692830012725,-15.7139900187849));
#12140=CARTESIAN_POINT('Ctrl Pts',(19.0653415301337,96.6842843394153,-18.0985520333781));
#12141=CARTESIAN_POINT('Ctrl Pts',(18.7887856820934,96.4256851402753,-18.9079119182639));
#12142=CARTESIAN_POINT('Ctrl Pts',(18.1273790350098,96.0834739774908,-20.493282275035));
#12143=CARTESIAN_POINT('Ctrl Pts',(17.742396615024,96.,-21.2692676147402));
#12144=CARTESIAN_POINT('Ctrl Pts',(16.8986195363537,96.,-22.7307323852593));
#12145=CARTESIAN_POINT('Ctrl Pts',(16.4190877291975,96.0834739774908,-23.45212961083));
#12146=CARTESIAN_POINT('Ctrl Pts',(15.3768200493689,96.4256851402753,-24.8176097478218));
#12147=CARTESIAN_POINT('Ctrl Pts',(14.8141717522739,96.6842843394153,-25.4617940802328));
#12148=CARTESIAN_POINT('Ctrl Pts',(13.0769954942976,97.692830012725,-27.2220405689019));
#12149=CARTESIAN_POINT('Ctrl Pts',(11.8489691987411,98.6870067773987,-28.1614978341941));
#12150=CARTESIAN_POINT('Ctrl Pts',(9.71353320304814,100.939132024555,-29.5291335226321));
#12151=CARTESIAN_POINT('Ctrl Pts',(8.64753200699724,102.36418544044,-30.0532001062722));
#12152=CARTESIAN_POINT('Ctrl Pts',(7.49579299781896,104.74529782815,-30.5469021730198));
#12153=CARTESIAN_POINT('Ctrl Pts',(7.18595457505932,105.58004369376,-30.6657861633899));
#12154=CARTESIAN_POINT('Ctrl Pts',(6.76887041885682,107.281307292478,-30.8210496511885));
#12155=CARTESIAN_POINT('Ctrl Pts',(6.66244658108837,108.148004216753,-30.8576723259829));
#12156=CARTESIAN_POINT('Ctrl Pts',(6.66244658108837,109.,-30.8576723259829));
#12157=CARTESIAN_POINT('',(-77.8262415816128,109.,47.9441085260903));
#12158=CARTESIAN_POINT('Origin',(61.9208163705871,109.,-47.7500000000002));
#12159=CARTESIAN_POINT('',(70.4208163705872,109.,-33.0275681356648));
#12160=CARTESIAN_POINT('Origin',(-61.9208163705876,109.,-47.7499999999993));
#12161=CARTESIAN_POINT('',(-53.4208163705878,109.,-62.4724318643349));
#12162=CARTESIAN_POINT('Origin',(0.,123.,-11.9999999999999));
#12163=CARTESIAN_POINT('',(0.,123.,8.00000000000008));
#12164=CARTESIAN_POINT('Origin',(0.,123.,-11.9999999999999));
#12165=CARTESIAN_POINT('Origin',(0.,181.568542494924,-11.9999999999999));
#12166=CARTESIAN_POINT('',(-2.44929359829471E-15,181.568542494924,8.00000000000008));
#12167=CARTESIAN_POINT('',(-2.44929359829471E-15,181.568542494924,8.00000000000008));
#12168=CARTESIAN_POINT('Origin',(-4.30163536500389,122.280548232157,61.5));
#12169=CARTESIAN_POINT('',(-4.30163536500389,122.280548232157,61.5));
#12170=CARTESIAN_POINT('Origin',(-5.2413279857898,121.938528088831,61.5));
#12171=CARTESIAN_POINT('',(-5.2413279857898,121.938528088831,65.5));
#12172=CARTESIAN_POINT('Origin',(-39.8034064033113,109.35896031048,0.));
#12173=CARTESIAN_POINT('Origin',(13.6521098277345,106.085051387833,61.5));
#12174=CARTESIAN_POINT('',(13.6521098277345,106.085051387833,61.5));
#12175=CARTESIAN_POINT('Origin',(13.8257580054015,107.069859140845,61.5));
#12176=CARTESIAN_POINT('',(13.8257580054015,107.069859140845,65.5));
#12177=CARTESIAN_POINT('Origin',(20.2125719494813,143.291280947184,0.));
#12178=CARTESIAN_POINT('Origin',(-9.35047446273056,98.6344003800105,61.5));
#12179=CARTESIAN_POINT('',(-9.35047446273056,98.6344003800105,61.5));
#12180=CARTESIAN_POINT('Origin',(-8.58443001961159,97.9916127703239,61.5));
#12181=CARTESIAN_POINT('',(-8.58443001961159,97.9916127703239,65.5));
#12182=CARTESIAN_POINT('Origin',(19.5908344538299,74.3497587423363,0.));
#12183=CARTESIAN_POINT('Origin',(56.8268122642887,106.085051387833,-60.5730739260735));
#12184=CARTESIAN_POINT('',(56.8268122642887,106.085051387833,-60.5730739260735));
#12185=CARTESIAN_POINT('Origin',(56.7399881754552,107.069859140845,-60.7234576592539));
#12186=CARTESIAN_POINT('',(60.204089790593,107.069859140845,-62.7234576592539));
#12187=CARTESIAN_POINT('Origin',(0.286018870672457,143.291280947184,-35.5046007840714));
#12188=CARTESIAN_POINT('Origin',(68.3281044095213,98.6344003800105,-40.6522515778379));
#12189=CARTESIAN_POINT('',(68.3281044095213,98.6344003800105,-40.6522515778379));
#12190=CARTESIAN_POINT('Origin',(67.9450821879618,97.991612770324,-41.3156655260068));
#12191=CARTESIAN_POINT('',(71.4091838030996,97.991612770324,-43.3156655260069));
#12192=CARTESIAN_POINT('Origin',(0.596887618498113,74.3497587423363,-34.9661603183521));
#12193=CARTESIAN_POINT('Origin',(65.803684860658,122.280548232157,-45.0246744960893));
#12194=CARTESIAN_POINT('',(65.803684860658,122.280548232157,-45.0246744960893));
#12195=CARTESIAN_POINT('Origin',(66.2735311710509,121.938528088831,-44.2108768147399));
#12196=CARTESIAN_POINT('',(69.7376327861887,121.938528088831,-46.2108768147399));
#12197=CARTESIAN_POINT('Origin',(30.294008047069,109.35896031048,16.4707611024238));
#12198=CARTESIAN_POINT('Origin',(-70.4789220920237,106.085051387833,-36.9269260739259));
#12199=CARTESIAN_POINT('',(-70.4789220920237,106.085051387833,-36.9269260739259));
#12200=CARTESIAN_POINT('Origin',(-70.5657461808571,107.069859140845,-36.7765423407455));
#12201=CARTESIAN_POINT('',(-74.0298477959949,107.069859140845,-38.7765423407454));
#12202=CARTESIAN_POINT('Origin',(-20.4985908201537,143.291280947184,-0.495399215928158));
#12203=CARTESIAN_POINT('Origin',(-58.9776299467913,98.6344003800105,-56.8477484221616));
#12204=CARTESIAN_POINT('',(-58.9776299467913,98.6344003800105,-56.8477484221616));
#12205=CARTESIAN_POINT('Origin',(-59.3606521683508,97.9916127703239,-56.1843344739927));
#12206=CARTESIAN_POINT('',(-62.8247537834886,97.9916127703239,-58.1843344739927));
#12207=CARTESIAN_POINT('Origin',(-20.1877220723281,74.3497587423363,-1.03383968164755));
#12208=CARTESIAN_POINT('Origin',(-61.5020494956546,122.280548232157,-52.4753255039102));
#12209=CARTESIAN_POINT('',(-61.5020494956546,122.280548232157,-52.4753255039102));
#12210=CARTESIAN_POINT('Origin',(-61.0322031852617,121.938528088831,-53.2891231852596));
#12211=CARTESIAN_POINT('',(-64.4963048003994,121.938528088831,-55.2891231852596));
#12212=CARTESIAN_POINT('Origin',(9.5093983562421,109.35896031048,-52.4707611024238));
#12213=CARTESIAN_POINT('',(0.,0.,0.));
#12214=CARTESIAN_POINT('Origin',(-102.211351574804,130.535898384862,-71.0117513459462));
#12215=CARTESIAN_POINT('',(-100.365693618373,135.788854382,-72.0117513459462));
#12216=CARTESIAN_POINT('Origin',(-103.943402382373,134.,-72.0117513459462));
#12217=CARTESIAN_POINT('',(-98.6336428108046,132.324752766862,-71.0117513459462));
#12218=CARTESIAN_POINT('',(-98.6336428108046,132.324752766862,-71.0117513459462));
#12219=CARTESIAN_POINT('Origin',(-102.211351574804,130.535898384862,-71.0117513459462));
#12220=CARTESIAN_POINT('Origin',(-102.211351574804,130.535898384862,-71.0117513459462));
#12221=CARTESIAN_POINT('',(-99.0808564063046,132.101145969112,-71.0117513459462));
#12222=CARTESIAN_POINT('Origin',(-102.211351574804,130.535898384862,-71.0117513459462));
#12223=CARTESIAN_POINT('Origin',(-103.943402382373,134.,-72.0117513459462));
#12224=CARTESIAN_POINT('',(-102.333433438573,134.8049844719,-72.0117513459462));
#12225=CARTESIAN_POINT('Origin',(-103.943402382373,134.,-72.0117513459462));
#12226=CARTESIAN_POINT('Origin',(-103.943402382373,134.,-72.0117513459462));
#12227=CARTESIAN_POINT('',(-100.107328997228,128.340314409459,-70.2617513459462));
#12228=CARTESIAN_POINT('Origin',(-100.912313469128,127.937822173509,-70.2617513459462));
#12229=CARTESIAN_POINT('',(-102.74870647877,133.623069372544,-71.7867513459462));
#12230=CARTESIAN_POINT('',(-103.138417910473,134.40249223595,-72.0117513459462));
#12231=CARTESIAN_POINT('Origin',(-103.55369095067,133.220577136594,-71.7867513459462));
#12232=CARTESIAN_POINT('Origin',(-103.943402382373,134.,-72.0117513459462));
#12233=CARTESIAN_POINT('',(-102.333433438573,134.8049844719,-72.0117513459462));
#12234=CARTESIAN_POINT('Origin',(-100.912313469128,127.937822173509,-70.2617513459462));
#12235=CARTESIAN_POINT('',(-97.7818183006279,129.503069757759,-70.2617513459462));
#12236=CARTESIAN_POINT('Origin',(-100.912313469128,127.937822173509,-70.2617513459462));
#12237=CARTESIAN_POINT('Origin',(-100.912313469128,127.937822173509,-70.2617513459462));
#12238=CARTESIAN_POINT('',(-97.7818183006279,129.503069757759,-70.2617513459462));
#12239=CARTESIAN_POINT('',(0.,0.,0.));
#12240=CARTESIAN_POINT('Origin',(-116.12807069331,130.343145750508,-79.0465728752519));
#12241=CARTESIAN_POINT('',(-115.553844652019,135.790187558086,-80.460786437625));
#12242=CARTESIAN_POINT('Origin',(-118.577560436093,133.171572875254,-80.460786437625));
#12243=CARTESIAN_POINT('',(-113.104354909236,132.96176043334,-79.0465728752519));
#12244=CARTESIAN_POINT('',(-113.104354909236,132.96176043334,-79.0465728752519));
#12245=CARTESIAN_POINT('Origin',(-116.12807069331,130.343145750508,-79.0465728752519));
#12246=CARTESIAN_POINT('Origin',(-116.12807069331,130.343145750508,-79.0465728752519));
#12247=CARTESIAN_POINT('',(-113.482319382245,132.634433597986,-79.0465728752519));
#12248=CARTESIAN_POINT('Origin',(-116.12807069331,130.343145750508,-79.0465728752519));
#12249=CARTESIAN_POINT('Origin',(-118.577560436093,133.171572875254,-80.460786437625));
#12250=CARTESIAN_POINT('',(-117.21688833326,134.349949482528,-80.460786437625));
#12251=CARTESIAN_POINT('Origin',(-118.577560436093,133.171572875254,-80.460786437625));
#12252=CARTESIAN_POINT('Origin',(-118.577560436093,133.171572875254,-80.460786437625));
#12253=CARTESIAN_POINT('',(-113.610617334806,128.811013710585,-77.9859127034721));
#12254=CARTESIAN_POINT('Origin',(-114.290953386223,128.221825406948,-77.9859127034721));
#12255=CARTESIAN_POINT('',(-117.34608919255,133.124365075823,-80.1425883860911));
#12256=CARTESIAN_POINT('',(-117.897224384677,133.760761178891,-80.460786437625));
#12257=CARTESIAN_POINT('Origin',(-118.026425243967,132.535176772186,-80.1425883860911));
#12258=CARTESIAN_POINT('Origin',(-118.577560436093,133.171572875254,-80.460786437625));
#12259=CARTESIAN_POINT('',(-117.21688833326,134.349949482528,-80.460786437625));
#12260=CARTESIAN_POINT('Origin',(-114.290953386223,128.221825406948,-77.9859127034721));
#12261=CARTESIAN_POINT('',(-111.645202075158,130.513113254426,-77.9859127034721));
#12262=CARTESIAN_POINT('Origin',(-114.290953386223,128.221825406948,-77.9859127034721));
#12263=CARTESIAN_POINT('Origin',(-114.290953386223,128.221825406948,-77.9859127034721));
#12264=CARTESIAN_POINT('',(-111.645202075158,130.513113254426,-77.9859127034721));
#12265=CARTESIAN_POINT('',(0.,0.,0.));
#12266=CARTESIAN_POINT('Origin',(-88.8998569762207,131.101020514434,-63.3263563561378));
#12267=CARTESIAN_POINT('',(-85.8999646576036,135.868902317108,-63.8439944463428));
#12268=CARTESIAN_POINT('Origin',(-89.7964324483888,134.96472381959,-63.8439944463428));
#12269=CARTESIAN_POINT('',(-85.0033891854356,132.005199011951,-63.3263563561378));
#12270=CARTESIAN_POINT('',(-85.0033891854356,132.005199011951,-63.3263563561378));
#12271=CARTESIAN_POINT('Origin',(-88.8998569762207,131.101020514434,-63.3263563561378));
#12272=CARTESIAN_POINT('Origin',(-88.8998569762207,131.101020514434,-63.3263563561378));
#12273=CARTESIAN_POINT('',(-85.4904476592837,131.892176699762,-63.3263563561378));
#12274=CARTESIAN_POINT('Origin',(-88.8998569762207,131.101020514434,-63.3263563561378));
#12275=CARTESIAN_POINT('Origin',(-89.7964324483888,134.96472381959,-63.8439944463428));
#12276=CARTESIAN_POINT('',(-88.0430219425354,135.371604143473,-63.8439944463428));
#12277=CARTESIAN_POINT('Origin',(-89.7964324483888,134.96472381959,-63.8439944463428));
#12278=CARTESIAN_POINT('Origin',(-89.7964324483888,134.96472381959,-63.8439944463428));
#12279=CARTESIAN_POINT('',(-87.350720119168,128.406683197508,-62.938127788484));
#12280=CARTESIAN_POINT('Origin',(-88.2274253720946,128.203243035566,-62.938127788484));
#12281=CARTESIAN_POINT('',(-88.7179977142243,134.298830737871,-63.7275258760467));
#12282=CARTESIAN_POINT('',(-88.9197271954621,135.168163981531,-63.8439944463428));
#12283=CARTESIAN_POINT('Origin',(-89.5947029671509,134.09539057593,-63.7275258760467));
#12284=CARTESIAN_POINT('Origin',(-89.7964324483888,134.96472381959,-63.8439944463428));
#12285=CARTESIAN_POINT('',(-88.0430219425354,135.371604143473,-63.8439944463428));
#12286=CARTESIAN_POINT('Origin',(-88.2274253720946,128.203243035566,-62.938127788484));
#12287=CARTESIAN_POINT('',(-84.8180160551577,128.994399220895,-62.938127788484));
#12288=CARTESIAN_POINT('Origin',(-88.2274253720946,128.203243035566,-62.938127788484));
#12289=CARTESIAN_POINT('Origin',(-88.2274253720946,128.203243035566,-62.938127788484));
#12290=CARTESIAN_POINT('',(-84.8180160551577,128.994399220895,-62.938127788484));
#12291=CARTESIAN_POINT('',(0.,0.,0.));
#12292=CARTESIAN_POINT('Origin',(-75.5607164801933,132.,-55.624999999998));
#12293=CARTESIAN_POINT('',(-75.5607164801933,136.,-59.6249999999981));
#12294=CARTESIAN_POINT('Origin',(-75.5607164801933,136.,-55.624999999998));
#12295=CARTESIAN_POINT('',(-75.5607164801933,132.,-59.6249999999981));
#12296=CARTESIAN_POINT('',(-75.5607164801933,132.,-59.6249999999981));
#12297=CARTESIAN_POINT('Origin',(-75.5607164801933,132.,-55.624999999998));
#12298=CARTESIAN_POINT('Origin',(-75.5607164801933,132.,-55.624999999998));
#12299=CARTESIAN_POINT('',(-75.5607164801933,132.,-59.1249999999981));
#12300=CARTESIAN_POINT('Origin',(-75.5607164801933,132.,-55.624999999998));
#12301=CARTESIAN_POINT('Origin',(-75.5607164801933,136.,-55.624999999998));
#12302=CARTESIAN_POINT('',(-75.5607164801933,136.,-57.424999999998));
#12303=CARTESIAN_POINT('Origin',(-75.5607164801933,136.,-55.624999999998));
#12304=CARTESIAN_POINT('Origin',(-75.5607164801933,136.,-55.624999999998));
#12305=CARTESIAN_POINT('',(-75.5607164801933,129.,-56.524999999998));
#12306=CARTESIAN_POINT('Origin',(-75.5607164801933,129.,-55.624999999998));
#12307=CARTESIAN_POINT('',(-75.5607164801933,135.1,-56.524999999998));
#12308=CARTESIAN_POINT('',(-75.5607164801933,136.,-56.524999999998));
#12309=CARTESIAN_POINT('Origin',(-75.5607164801933,135.1,-55.624999999998));
#12310=CARTESIAN_POINT('Origin',(-75.5607164801933,136.,-55.624999999998));
#12311=CARTESIAN_POINT('',(-75.5607164801933,136.,-57.424999999998));
#12312=CARTESIAN_POINT('Origin',(-75.5607164801933,129.,-55.624999999998));
#12313=CARTESIAN_POINT('',(-75.5607164801933,129.,-59.1249999999981));
#12314=CARTESIAN_POINT('Origin',(-75.5607164801933,129.,-55.624999999998));
#12315=CARTESIAN_POINT('Origin',(-75.5607164801933,129.,-55.624999999998));
#12316=CARTESIAN_POINT('',(-75.5607164801933,129.,-59.1249999999981));
#12317=CARTESIAN_POINT('',(0.,0.,0.));
#12318=CARTESIAN_POINT('Origin',(-69.7150450046476,109.,-52.2499999999992));
#12319=CARTESIAN_POINT('',(-57.0362860918569,101.937180526611,-60.2102546138697));
#12320=CARTESIAN_POINT('',(-60.5003877069947,101.937180526611,-62.2102546138697));
#12321=CARTESIAN_POINT('',(-60.5003877069947,101.937180526611,-62.2102546138697));
#12322=CARTESIAN_POINT('',(-63.4028671781572,123.991664350565,-49.1830127018903));
#12323=CARTESIAN_POINT('Origin',(-63.6528671781565,109.,-48.7499999999993));
#12324=CARTESIAN_POINT('',(-66.866968793295,123.991664350565,-51.1830127018903));
#12325=CARTESIAN_POINT('',(-66.866968793295,123.991664350565,-51.1830127018903));
#12326=CARTESIAN_POINT('Origin',(-67.1169687932943,109.,-50.7499999999993));
#12327=CARTESIAN_POINT('Origin',(-69.7150450046476,109.,-52.2499999999992));
#12328=CARTESIAN_POINT('',(-60.7503877069946,101.071155122826,-61.7772419119775));
#12329=CARTESIAN_POINT('',(-57.2862860918569,101.071155122826,-59.7772419119775));
#12330=CARTESIAN_POINT('',(-60.7503877069946,101.071155122826,-61.7772419119775));
#12331=CARTESIAN_POINT('',(-73.4835498795932,101.071155122824,-39.7227580880222));
#12332=CARTESIAN_POINT('Origin',(-67.1169687932943,109.,-50.7499999999993));
#12333=CARTESIAN_POINT('',(-70.0194482644555,101.071155122824,-37.7227580880222));
#12334=CARTESIAN_POINT('',(-73.4835498795932,101.071155122824,-39.7227580880221));
#12335=CARTESIAN_POINT('Origin',(-63.6528671781565,109.,-48.7499999999993));
#12336=CARTESIAN_POINT('Origin',(-119.078493020361,109.,-80.7499999999988));
#12337=CARTESIAN_POINT('',(-65.5747753124034,96.49269543419,-59.421157464004));
#12338=CARTESIAN_POINT('',(-73.855314696892,96.4926954341901,-45.0788425359943));
#12339=CARTESIAN_POINT('Origin',(-69.7150450046476,109.,-52.2499999999992));
#12340=CARTESIAN_POINT('',(-123.218762712605,96.4926954341901,-73.5788425359939));
#12341=CARTESIAN_POINT('',(-123.218762712605,96.4926954341901,-73.5788425359939));
#12342=CARTESIAN_POINT('',(-114.938223328117,96.49269543419,-87.9211574640035));
#12343=CARTESIAN_POINT('Origin',(-119.078493020361,109.,-80.7499999999988));
#12344=CARTESIAN_POINT('',(-114.938223328117,96.49269543419,-87.9211574640035));
#12345=CARTESIAN_POINT('Origin',(-119.078493020361,109.,-80.7499999999988));
#12346=CARTESIAN_POINT('',(-94.3860089394201,105.235685467736,-49.7275542973482));
#12347=CARTESIAN_POINT('',(-82.8207084929668,105.235685467736,-43.0503249713298));
#12348=CARTESIAN_POINT('',(-94.3860089394201,105.235685467737,-49.7275542973482));
#12349=CARTESIAN_POINT('',(-91.0176401746589,103.250749366077,-48.5513043322017));
#12350=CARTESIAN_POINT('Ctrl Pts',(-91.0176401746589,103.250749366077,-48.5513043322017));
#12351=CARTESIAN_POINT('Ctrl Pts',(-91.2361059276669,103.557750420993,-48.5303294493383));
#12352=CARTESIAN_POINT('Ctrl Pts',(-91.4832335600058,103.842139746856,-48.5508334265686));
#12353=CARTESIAN_POINT('Ctrl Pts',(-92.1066673879442,104.430592760333,-48.6750977465524));
#12354=CARTESIAN_POINT('Ctrl Pts',(-92.5431699718694,104.735168552794,-48.8223964645982));
#12355=CARTESIAN_POINT('Ctrl Pts',(-93.461912716518,105.137985045737,-49.2219363914119));
#12356=CARTESIAN_POINT('Ctrl Pts',(-93.9449426785634,105.235685467736,-49.4729045729122));
#12357=CARTESIAN_POINT('Ctrl Pts',(-94.3860089394201,105.235685467736,-49.7275542973483));
#12358=CARTESIAN_POINT('',(-92.3860089394197,98.3074822374609,-53.1916559124865));
#12359=CARTESIAN_POINT('Ctrl Pts',(-92.3860089394197,98.307482237461,-53.1916559124864));
#12360=CARTESIAN_POINT('Ctrl Pts',(-91.944942678563,98.307482237461,-52.9370061880504));
#12361=CARTESIAN_POINT('Ctrl Pts',(-91.5102607802988,98.3772644212952,-52.6022967036335));
#12362=CARTESIAN_POINT('Ctrl Pts',(-90.7942826050959,98.676845000861,-51.8515582405649));
#12363=CARTESIAN_POINT('Ctrl Pts',(-90.5123369230427,98.9076700218055,-51.4365591158164));
#12364=CARTESIAN_POINT('Ctrl Pts',(-90.1413389560881,99.4578375470661,-50.6726253387866));
#12365=CARTESIAN_POINT('Ctrl Pts',(-90.0255053791506,99.8112989429842,-50.2740223286365));
#12366=CARTESIAN_POINT('Ctrl Pts',(-89.9729277960154,100.614428273412,-49.573341944019));
#12367=CARTESIAN_POINT('Ctrl Pts',(-90.0353007740436,101.064744995698,-49.2720751413297));
#12368=CARTESIAN_POINT('Ctrl Pts',(-90.2865953679429,101.9352550043,-48.8368201370289));
#12369=CARTESIAN_POINT('Ctrl Pts',(-90.4922380489042,102.413371759201,-48.6738702011243));
#12370=CARTESIAN_POINT('Ctrl Pts',(-90.8440070426079,102.99654996933,-48.5751774684912));
#12371=CARTESIAN_POINT('Ctrl Pts',(-90.9285040512729,103.125489990024,-48.559862285662));
#12372=CARTESIAN_POINT('Ctrl Pts',(-91.0176401746589,103.250749366077,-48.5513043322017));
#12373=CARTESIAN_POINT('',(-80.8207084929665,98.3074822374608,-46.5144265864682));
#12374=CARTESIAN_POINT('',(-92.3860089394198,98.3074822374611,-53.1916559124864));
#12375=CARTESIAN_POINT('',(-84.4784050214276,104.702740240336,-44.1791103605043));
#12376=CARTESIAN_POINT('Ctrl Pts',(-84.4784050214273,104.702740240336,-44.179110360504));
#12377=CARTESIAN_POINT('Ctrl Pts',(-84.719910157753,104.526945752297,-44.3792409314819));
#12378=CARTESIAN_POINT('Ctrl Pts',(-84.9292227283709,104.313493521274,-44.5780840276366));
#12379=CARTESIAN_POINT('Ctrl Pts',(-85.3433081511931,103.743726568118,-45.0453786543482));
#12380=CARTESIAN_POINT('Ctrl Pts',(-85.5286602574863,103.319666529342,-45.3392616445606));
#12381=CARTESIAN_POINT('Ctrl Pts',(-85.6804888744289,102.416155145618,-45.8942563092267));
#12382=CARTESIAN_POINT('Ctrl Pts',(-85.6462202716666,101.937209973523,-46.1563950132377));
#12383=CARTESIAN_POINT('Ctrl Pts',(-85.3937969757602,101.062790026475,-46.5936049867616));
#12384=CARTESIAN_POINT('Ctrl Pts',(-85.1596379659028,100.611874672147,-46.7963965459624));
#12385=CARTESIAN_POINT('Ctrl Pts',(-84.5153961509797,99.8096167014324,-47.0942865585158));
#12386=CARTESIAN_POINT('Ctrl Pts',(-84.1059621410022,99.4574342557325,-47.1885248105415));
#12387=CARTESIAN_POINT('Ctrl Pts',(-83.2575101221815,98.9126166677475,-47.2430172368065));
#12388=CARTESIAN_POINT('Ctrl Pts',(-82.7609372275344,98.6829050367047,-47.2068324926174));
#12389=CARTESIAN_POINT('Ctrl Pts',(-81.7609021788356,98.3807025943171,-46.9694819795316));
#12390=CARTESIAN_POINT('Ctrl Pts',(-81.2579982865691,98.3074822374608,-46.7668959665184));
#12391=CARTESIAN_POINT('Ctrl Pts',(-80.8207084929665,98.3074822374608,-46.5144265864681));
#12392=CARTESIAN_POINT('Ctrl Pts',(-82.8207084929668,105.235685467736,-43.0503249713298));
#12393=CARTESIAN_POINT('Ctrl Pts',(-83.2579982865694,105.235685467736,-43.3027943513801));
#12394=CARTESIAN_POINT('Ctrl Pts',(-83.7101950061769,105.133251025885,-43.5932077637468));
#12395=CARTESIAN_POINT('Ctrl Pts',(-84.2375848518395,104.864030249166,-43.985328869011));
#12396=CARTESIAN_POINT('Ctrl Pts',(-84.3616836412502,104.787703134226,-44.0823856414543));
#12397=CARTESIAN_POINT('Ctrl Pts',(-84.4784050214273,104.702740240336,-44.179110360504));
#12398=CARTESIAN_POINT('Origin',(-119.078493020361,109.,-80.7499999999988));
#12399=CARTESIAN_POINT('',(-105.931810542547,105.235685467737,-56.3935259609235));
#12400=CARTESIAN_POINT('',(-105.931810542547,105.235685467737,-56.3935259609236));
#12401=CARTESIAN_POINT('',(-102.208219994794,103.102717662028,-55.0841964154936));
#12402=CARTESIAN_POINT('Ctrl Pts',(-102.208219994794,103.102717662026,-55.0841964154936));
#12403=CARTESIAN_POINT('Ctrl Pts',(-102.449021592923,103.452288080539,-55.0506293513879));
#12404=CARTESIAN_POINT('Ctrl Pts',(-102.730142130046,103.775612080798,-55.0719387240821));
#12405=CARTESIAN_POINT('Ctrl Pts',(-103.427690853637,104.41668799164,-55.2155771708353));
#12406=CARTESIAN_POINT('Ctrl Pts',(-103.909507673844,104.73291730259,-55.385468864601));
#12407=CARTESIAN_POINT('Ctrl Pts',(-104.920531073176,105.142197830513,-55.8362211929756));
#12408=CARTESIAN_POINT('Ctrl Pts',(-105.450263434612,105.235685467736,-56.1155046085297));
#12409=CARTESIAN_POINT('Ctrl Pts',(-105.931810542547,105.235685467736,-56.3935259609236));
#12410=CARTESIAN_POINT('',(-103.931810542547,98.307482237461,-59.8576275760617));
#12411=CARTESIAN_POINT('Ctrl Pts',(-103.931810542547,98.3074822374611,-59.8576275760617));
#12412=CARTESIAN_POINT('Ctrl Pts',(-103.450263434612,98.3074822374611,-59.5796062236677));
#12413=CARTESIAN_POINT('Ctrl Pts',(-102.966762319561,98.3741443355121,-59.2202479404765));
#12414=CARTESIAN_POINT('Ctrl Pts',(-102.161749770577,98.6785063270139,-58.4126743523891));
#12415=CARTESIAN_POINT('Ctrl Pts',(-101.840308730574,98.9178350152992,-57.9650036590062));
#12416=CARTESIAN_POINT('Ctrl Pts',(-101.440098436538,99.4841271059821,-57.1713087801904));
#12417=CARTESIAN_POINT('Ctrl Pts',(-101.317391802105,99.8312991080725,-56.7758910574572));
#12418=CARTESIAN_POINT('Ctrl Pts',(-101.255012945074,100.623349028226,-56.0804534046886));
#12419=CARTESIAN_POINT('Ctrl Pts',(-101.314116564966,101.068801289505,-55.7811982784879));
#12420=CARTESIAN_POINT('Ctrl Pts',(-101.563069256545,101.931198710494,-55.3499995679935));
#12421=CARTESIAN_POINT('Ctrl Pts',(-101.769030711735,102.403958803925,-55.1901485168392));
#12422=CARTESIAN_POINT('Ctrl Pts',(-102.095779742704,102.93486881927,-55.1031827978842));
#12423=CARTESIAN_POINT('Ctrl Pts',(-102.150902897407,103.019510732018,-55.0921862573272));
#12424=CARTESIAN_POINT('Ctrl Pts',(-102.208219994794,103.102717662026,-55.0841964154936));
#12425=CARTESIAN_POINT('',(-103.931810542547,98.3074822374611,-59.8576275760617));
#12426=CARTESIAN_POINT('Ctrl Pts',(-94.3860089394201,105.235685467736,-49.7275542973483));
#12427=CARTESIAN_POINT('Ctrl Pts',(-94.8437110509037,105.235685467736,-49.991808734622));
#12428=CARTESIAN_POINT('Ctrl Pts',(-95.3183294965658,105.131719766023,-50.2956435885911));
#12429=CARTESIAN_POINT('Ctrl Pts',(-96.1649446403336,104.726122671488,-50.9165050382747));
#12430=CARTESIAN_POINT('Ctrl Pts',(-96.5365223340826,104.425439262705,-51.2347212917227));
#12431=CARTESIAN_POINT('Ctrl Pts',(-97.079067270285,103.751330105903,-51.8179767152385));
#12432=CARTESIAN_POINT('Ctrl Pts',(-97.2914477713889,103.33295780308,-52.124268380383));
#12433=CARTESIAN_POINT('Ctrl Pts',(-97.4838471817179,102.430163538116,-52.7010684635898));
#12434=CARTESIAN_POINT('Ctrl Pts',(-97.4623083504636,101.946025606973,-52.9725395573328));
#12435=CARTESIAN_POINT('Ctrl Pts',(-97.2047953462119,101.053974393026,-53.4185651643064));
#12436=CARTESIAN_POINT('Ctrl Pts',(-96.9552287340129,100.59897551963,-53.616662472833));
#12437=CARTESIAN_POINT('Ctrl Pts',(-96.2710769848093,99.7982897132515,-53.8916024252977));
#12438=CARTESIAN_POINT('Ctrl Pts',(-95.8377694343555,99.451348267594,-53.9679676343933));
#12439=CARTESIAN_POINT('Ctrl Pts',(-94.9448662844064,98.9117809702792,-53.991550437936));
#12440=CARTESIAN_POINT('Ctrl Pts',(-94.4206402272791,98.683674936935,-53.9377289055515));
#12441=CARTESIAN_POINT('Ctrl Pts',(-93.3698028357836,98.3818254132703,-53.670590764968));
#12442=CARTESIAN_POINT('Ctrl Pts',(-92.8437110509033,98.307482237461,-53.4559103497602));
#12443=CARTESIAN_POINT('Ctrl Pts',(-92.3860089394197,98.307482237461,-53.1916559124864));
#12444=CARTESIAN_POINT('Origin',(-119.078493020361,109.,-80.7499999999988));
#12445=CARTESIAN_POINT('',(-117.424340315019,105.235685467737,-63.0287411187298));
#12446=CARTESIAN_POINT('',(-117.424340315019,105.235685467737,-63.0287411187298));
#12447=CARTESIAN_POINT('',(-112.873099678569,102.847499823892,-61.3708278876974));
#12448=CARTESIAN_POINT('Ctrl Pts',(-112.873099678569,102.847499823892,-61.3708278876974));
#12449=CARTESIAN_POINT('Ctrl Pts',(-112.885263071986,102.865530125643,-61.3684870415431));
#12450=CARTESIAN_POINT('Ctrl Pts',(-112.897548248638,102.883504310233,-61.366295141775));
#12451=CARTESIAN_POINT('Ctrl Pts',(-113.223445655223,103.354153784421,-61.312605698808));
#12452=CARTESIAN_POINT('Ctrl Pts',(-113.617943081627,103.765699546249,-61.3609453836262));
#12453=CARTESIAN_POINT('Ctrl Pts',(-114.51341914509,104.46875863804,-61.596335766007));
#12454=CARTESIAN_POINT('Ctrl Pts',(-115.084650741731,104.772419738951,-61.8242044014969));
#12455=CARTESIAN_POINT('Ctrl Pts',(-116.26458534071,105.155153282331,-62.3819677418281));
#12456=CARTESIAN_POINT('Ctrl Pts',(-116.873387883958,105.235685467737,-62.7106485843461));
#12457=CARTESIAN_POINT('Ctrl Pts',(-117.424340315019,105.235685467736,-63.0287411187299));
#12458=CARTESIAN_POINT('',(-115.424340315019,98.3074822374612,-66.4928427338677));
#12459=CARTESIAN_POINT('Ctrl Pts',(-115.424340315019,98.3074822374612,-66.4928427338678));
#12460=CARTESIAN_POINT('Ctrl Pts',(-114.873387883957,98.3074822374612,-66.1747501994839));
#12461=CARTESIAN_POINT('Ctrl Pts',(-114.304395627967,98.3648569324462,-65.7771159167707));
#12462=CARTESIAN_POINT('Ctrl Pts',(-113.316922034078,98.6488278676478,-64.8860003371488));
#12463=CARTESIAN_POINT('Ctrl Pts',(-112.899248494017,98.8771074785532,-64.3921613457507));
#12464=CARTESIAN_POINT('Ctrl Pts',(-112.369176942676,99.4398467473837,-63.5238717830588));
#12465=CARTESIAN_POINT('Ctrl Pts',(-112.191730388089,99.7801872611806,-63.0995889604281));
#12466=CARTESIAN_POINT('Ctrl Pts',(-112.057561335007,100.581884791004,-62.3492963885222));
#12467=CARTESIAN_POINT('Ctrl Pts',(-112.099359165682,101.044133890221,-62.0245059301422));
#12468=CARTESIAN_POINT('Ctrl Pts',(-112.357346552702,101.937828414283,-61.5776586681113));
#12469=CARTESIAN_POINT('Ctrl Pts',(-112.577858013516,102.409850877713,-61.4276471726289));
#12470=CARTESIAN_POINT('Ctrl Pts',(-112.873099678569,102.847499823891,-61.3708278876975));
#12471=CARTESIAN_POINT('',(-115.424340315019,98.3074822374611,-66.4928427338679));
#12472=CARTESIAN_POINT('Ctrl Pts',(-105.931810542547,105.235685467736,-56.3935259609236));
#12473=CARTESIAN_POINT('Ctrl Pts',(-106.441097653729,105.235685467736,-56.687563011659));
#12474=CARTESIAN_POINT('Ctrl Pts',(-106.974640486628,105.132960205187,-57.0250658019486));
#12475=CARTESIAN_POINT('Ctrl Pts',(-107.947581410815,104.730808636537,-57.7176366639949));
#12476=CARTESIAN_POINT('Ctrl Pts',(-108.386686426508,104.432320373104,-58.0736604657704));
#12477=CARTESIAN_POINT('Ctrl Pts',(-109.030432576161,103.765790736202,-58.7123084319066));
#12478=CARTESIAN_POINT('Ctrl Pts',(-109.294438065739,103.359086193815,-59.0420063444297));
#12479=CARTESIAN_POINT('Ctrl Pts',(-109.56709842014,102.458977333711,-59.6612621436709));
#12480=CARTESIAN_POINT('Ctrl Pts',(-109.572926265459,101.965344390994,-59.9517288812603));
#12481=CARTESIAN_POINT('Ctrl Pts',(-109.304259556052,101.034655609004,-60.4170732722551));
#12482=CARTESIAN_POINT('Ctrl Pts',(-109.022522963702,100.572512615502,-60.6044945027757));
#12483=CARTESIAN_POINT('Ctrl Pts',(-108.260113770694,99.7760817327768,-60.8335085749491));
#12484=CARTESIAN_POINT('Ctrl Pts',(-107.781619042588,99.4397737575475,-60.8753169212342));
#12485=CARTESIAN_POINT('Ctrl Pts',(-106.791454021988,98.9062732240887,-60.8366840402783));
#12486=CARTESIAN_POINT('Ctrl Pts',(-106.200906509653,98.6801492903,-60.7429663371135));
#12487=CARTESIAN_POINT('Ctrl Pts',(-105.025500473564,98.3809411378044,-60.40107533564));
#12488=CARTESIAN_POINT('Ctrl Pts',(-104.441097653728,98.3074822374611,-60.1516646267969));
#12489=CARTESIAN_POINT('Ctrl Pts',(-103.931810542547,98.3074822374611,-59.8576275760616));
#12490=CARTESIAN_POINT('Origin',(-119.078493020361,109.,-80.7499999999988));
#12491=CARTESIAN_POINT('',(-118.78998649473,98.3074822374612,-68.4359994617213));
#12492=CARTESIAN_POINT('',(-118.78998649473,98.3074822374611,-68.4359994617214));
#12493=CARTESIAN_POINT('Ctrl Pts',(-117.424340315019,105.235685467736,-63.0287411187299));
#12494=CARTESIAN_POINT('Ctrl Pts',(-118.104455067791,105.235685467737,-63.4214055543222));
#12495=CARTESIAN_POINT('Ctrl Pts',(-118.823383370921,105.115025708115,-63.8707727019096));
#12496=CARTESIAN_POINT('Ctrl Pts',(-120.152211057545,104.638615075121,-64.7952439254207));
#12497=CARTESIAN_POINT('Ctrl Pts',(-120.762708154872,104.285378551405,-65.27078272247));
#12498=CARTESIAN_POINT('Ctrl Pts',(-121.530321038309,103.561110088859,-66.0199577490771));
#12499=CARTESIAN_POINT('Ctrl Pts',(-121.807474740758,103.201357059968,-66.343360523086));
#12500=CARTESIAN_POINT('Ctrl Pts',(-122.043414724861,102.594072465734,-66.7981024939494));
#12501=CARTESIAN_POINT('Ctrl Pts',(-122.092678493038,102.380375656682,-66.945003657385));
#12502=CARTESIAN_POINT('Ctrl Pts',(-122.117297884372,101.943528113597,-67.2175789887018));
#12503=CARTESIAN_POINT('Ctrl Pts',(-122.092529257229,101.720365047742,-67.3432446008741));
#12504=CARTESIAN_POINT('Ctrl Pts',(-121.965301437595,101.279634952257,-67.5636096486164));
#12505=CARTESIAN_POINT('Ctrl Pts',(-121.863134141106,101.063079080039,-67.6578035054809));
#12506=CARTESIAN_POINT('Ctrl Pts',(-121.5934173484,100.650884319169,-67.8097493261416));
#12507=CARTESIAN_POINT('Ctrl Pts',(-121.425973083727,100.45519187943,-67.8675427871017));
#12508=CARTESIAN_POINT('Ctrl Pts',(-120.858109129937,99.9126581141667,-67.9877099959866));
#12509=CARTESIAN_POINT('Ctrl Pts',(-120.389803254753,99.6102405927516,-67.9953924971306));
#12510=CARTESIAN_POINT('Ctrl Pts',(-119.242323386653,99.0186112201875,-67.9041663880787));
#12511=CARTESIAN_POINT('Ctrl Pts',(-118.452225355267,98.7496918581534,-67.7397055339048));
#12512=CARTESIAN_POINT('Ctrl Pts',(-116.883055382911,98.393532390957,-67.231519360489));
#12513=CARTESIAN_POINT('Ctrl Pts',(-116.10445506779,98.3074822374612,-66.8855071694601));
#12514=CARTESIAN_POINT('Ctrl Pts',(-115.424340315019,98.3074822374612,-66.4928427338678));
#12515=CARTESIAN_POINT('',(-120.78998649473,105.235685467737,-64.9718978465832));
#12516=CARTESIAN_POINT('',(-120.78998649473,105.235685467737,-64.9718978465831));
#12517=CARTESIAN_POINT('Ctrl Pts',(-118.78998649473,98.3074822374612,-68.4359994617213));
#12518=CARTESIAN_POINT('Ctrl Pts',(-118.918348276834,98.3074822374612,-68.5101091711724));
#12519=CARTESIAN_POINT('Ctrl Pts',(-119.051966028522,98.319606062948,-68.5729797213706));
#12520=CARTESIAN_POINT('Ctrl Pts',(-119.390180292013,98.3776312711511,-68.7006060360938));
#12521=CARTESIAN_POINT('Ctrl Pts',(-119.594844068455,98.4360499331429,-68.7509667466566));
#12522=CARTESIAN_POINT('Ctrl Pts',(-120.108561068232,98.6351217911646,-68.822841039124));
#12523=CARTESIAN_POINT('Ctrl Pts',(-120.410333239601,98.8023575570841,-68.8132768624661));
#12524=CARTESIAN_POINT('Ctrl Pts',(-121.095658711484,99.2862798538955,-68.7087637376292));
#12525=CARTESIAN_POINT('Ctrl Pts',(-121.453647702316,99.6436546824008,-68.5719722406892));
#12526=CARTESIAN_POINT('Ctrl Pts',(-121.95322023847,100.313709548206,-68.2828712619504));
#12527=CARTESIAN_POINT('Ctrl Pts',(-122.13026373805,100.619480486203,-68.1403943115824));
#12528=CARTESIAN_POINT('Ctrl Pts',(-122.350414930589,101.118875846441,-67.8997101912188));
#12529=CARTESIAN_POINT('Ctrl Pts',(-122.419254299142,101.308117977183,-67.8067240343058));
#12530=CARTESIAN_POINT('Ctrl Pts',(-122.529732701345,101.690626616667,-67.6154765320548));
#12531=CARTESIAN_POINT('Ctrl Pts',(-122.571615353665,101.884694244957,-67.5168156573903));
#12532=CARTESIAN_POINT('Ctrl Pts',(-122.647401154913,102.409372784178,-67.2455011686517));
#12533=CARTESIAN_POINT('Ctrl Pts',(-122.655932486104,102.745023337843,-67.0673187398412));
#12534=CARTESIAN_POINT('Ctrl Pts',(-122.572273917842,103.513663673561,-66.6372167411127));
#12535=CARTESIAN_POINT('Ctrl Pts',(-122.443353045988,103.95119638048,-66.3765548091624));
#12536=CARTESIAN_POINT('Ctrl Pts',(-122.075417244245,104.56927639081,-65.9299074078767));
#12537=CARTESIAN_POINT('Ctrl Pts',(-121.885875205944,104.790787749988,-65.7451136026938));
#12538=CARTESIAN_POINT('Ctrl Pts',(-121.506987477856,105.058995953627,-65.4396037944961));
#12539=CARTESIAN_POINT('Ctrl Pts',(-121.342237738227,105.139116769073,-65.3199491226463));
#12540=CARTESIAN_POINT('Ctrl Pts',(-121.043690674034,105.218909586375,-65.1233635722866));
#12541=CARTESIAN_POINT('Ctrl Pts',(-120.918381560469,105.235685467737,-65.0460267723497));
#12542=CARTESIAN_POINT('Ctrl Pts',(-120.78998649473,105.235685467737,-64.9718978465831));
#12543=CARTESIAN_POINT('Origin',(-119.078493020361,109.,-80.7499999999988));
#12544=CARTESIAN_POINT('',(-66.3693581073396,122.42480974691,-58.0448996923544));
#12545=CARTESIAN_POINT('',(-62.2290884150953,108.0824948189,-65.2160571563592));
#12546=CARTESIAN_POINT('Origin',(-69.7150450046476,109.,-52.2499999999992));
#12547=CARTESIAN_POINT('',(-111.592536430809,108.0824948189,-93.7160571563587));
#12548=CARTESIAN_POINT('',(-111.592536430809,108.0824948189,-93.7160571563587));
#12549=CARTESIAN_POINT('',(-115.732806123053,122.42480974691,-86.5448996923539));
#12550=CARTESIAN_POINT('Origin',(-119.078493020361,109.,-80.7499999999988));
#12551=CARTESIAN_POINT('',(-115.732806123053,122.42480974691,-86.5448996923539));
#12552=CARTESIAN_POINT('Origin',(-119.078493020361,109.,-80.7499999999988));
#12553=CARTESIAN_POINT('',(-81.8660249138711,98.3074822374625,-71.4128027395503));
#12554=CARTESIAN_POINT('',(-70.3007244674178,98.3074822374627,-64.7355734135318));
#12555=CARTESIAN_POINT('',(-81.8660249138712,98.3074822374623,-71.4128027395501));
#12556=CARTESIAN_POINT('',(-78.1372951281693,99.8763092742309,-70.8607163717404));
#12557=CARTESIAN_POINT('Ctrl Pts',(-78.1372951281693,99.8763092742309,-70.8607163717404));
#12558=CARTESIAN_POINT('Ctrl Pts',(-78.3931479940217,99.6124791386442,-70.7749851098822));
#12559=CARTESIAN_POINT('Ctrl Pts',(-78.6840646784847,99.3786530548441,-70.7196442240182));
#12560=CARTESIAN_POINT('Ctrl Pts',(-79.4092304936657,98.9076700218071,-70.6677035733428));
#12561=CARTESIAN_POINT('Ctrl Pts',(-79.9096031192728,98.6768450008626,-70.704376134114));
#12562=CARTESIAN_POINT('Ctrl Pts',(-80.9177507874897,98.3772644212968,-70.9490621908606));
#12563=CARTESIAN_POINT('Ctrl Pts',(-81.4249586530144,98.3074822374626,-71.1581530151143));
#12564=CARTESIAN_POINT('Ctrl Pts',(-81.8660249138711,98.3074822374626,-71.4128027395504));
#12565=CARTESIAN_POINT('',(-79.8660249138713,105.235685467738,-74.8769043546876));
#12566=CARTESIAN_POINT('Ctrl Pts',(-79.8660249138713,105.235685467738,-74.8769043546876));
#12567=CARTESIAN_POINT('Ctrl Pts',(-79.4249586530146,105.235685467738,-74.6222546302515));
#12568=CARTESIAN_POINT('Ctrl Pts',(-78.966098851271,105.13798504574,-74.3294225030814));
#12569=CARTESIAN_POINT('Ctrl Pts',(-78.1607157524998,104.735168552796,-73.7335379100799));
#12570=CARTESIAN_POINT('Ctrl Pts',(-77.8149000287647,104.430592760335,-73.4291649426061));
#12571=CARTESIAN_POINT('Ctrl Pts',(-77.3250662827369,103.743205497,-72.8710607726881));
#12572=CARTESIAN_POINT('Ctrl Pts',(-77.1468233216009,103.317679951548,-72.580553986839));
#12573=CARTESIAN_POINT('Ctrl Pts',(-77.0066222737195,102.413371759203,-72.0316418950969));
#12574=CARTESIAN_POINT('Ctrl Pts',(-77.0449197172773,101.935255004302,-71.7720751413298));
#12575=CARTESIAN_POINT('Ctrl Pts',(-77.2962143111765,101.0647449957,-71.3368201370292));
#12576=CARTESIAN_POINT('Ctrl Pts',(-77.5259325266081,100.614428273414,-71.1321701522025));
#12577=CARTESIAN_POINT('Ctrl Pts',(-77.9342089099037,100.096499176469,-70.9356037497933));
#12578=CARTESIAN_POINT('Ctrl Pts',(-78.0329047040169,99.9839545009761,-70.895695549162));
#12579=CARTESIAN_POINT('Ctrl Pts',(-78.1372951281693,99.8763092742309,-70.8607163717404));
#12580=CARTESIAN_POINT('',(-68.3007244674181,105.235685467739,-68.1996750286692));
#12581=CARTESIAN_POINT('',(-79.8660249138713,105.235685467738,-74.8769043546876));
#12582=CARTESIAN_POINT('',(-71.8391803616632,98.7027402403375,-66.0708896394943));
#12583=CARTESIAN_POINT('Ctrl Pts',(-71.8391803616628,98.7027402403373,-66.070889639494));
#12584=CARTESIAN_POINT('Ctrl Pts',(-72.0439884445282,98.8361606209892,-66.3345813715533));
#12585=CARTESIAN_POINT('Ctrl Pts',(-72.2115336533623,99.001384056873,-66.6057676604154));
#12586=CARTESIAN_POINT('Ctrl Pts',(-72.5271374781293,99.4574342557344,-67.2436374185692));
#12587=CARTESIAN_POINT('Ctrl Pts',(-72.6502417628557,99.8096167014344,-67.645336798396));
#12588=CARTESIAN_POINT('Ctrl Pts',(-72.7143823519123,100.611874672149,-68.3522115825761));
#12589=CARTESIAN_POINT('Ctrl Pts',(-72.6558392149002,101.062790026477,-68.6563950132379));
#12590=CARTESIAN_POINT('Ctrl Pts',(-72.4034159189938,101.937209973525,-69.0936049867617));
#12591=CARTESIAN_POINT('Ctrl Pts',(-72.1935314433864,102.41615514562,-69.2543518193115));
#12592=CARTESIAN_POINT('Ctrl Pts',(-71.6369776563495,103.319666529344,-69.4003617123507));
#12593=CARTESIAN_POINT('Ctrl Pts',(-71.2897914679388,103.743726568121,-69.3867835747619));
#12594=CARTESIAN_POINT('Ctrl Pts',(-70.5589898894586,104.424395182907,-69.2374994608244));
#12595=CARTESIAN_POINT('Ctrl Pts',(-70.1256610955174,104.727134811084,-69.0917727209338));
#12596=CARTESIAN_POINT('Ctrl Pts',(-69.2156180135337,105.133251025888,-68.6985515492242));
#12597=CARTESIAN_POINT('Ctrl Pts',(-68.7380142610207,105.235685467739,-68.4521444087194));
#12598=CARTESIAN_POINT('Ctrl Pts',(-68.3007244674181,105.235685467739,-68.1996750286692));
#12599=CARTESIAN_POINT('Ctrl Pts',(-70.3007244674178,98.3074822374626,-64.7355734135318));
#12600=CARTESIAN_POINT('Ctrl Pts',(-70.7380142610204,98.3074822374626,-64.9880427935821));
#12601=CARTESIAN_POINT('Ctrl Pts',(-71.1649108408744,98.3807025943189,-65.3222773334404));
#12602=CARTESIAN_POINT('Ctrl Pts',(-71.63264360737,98.5810373096057,-65.817727530853));
#12603=CARTESIAN_POINT('Ctrl Pts',(-71.7401949633927,98.6382570943041,-65.9434452986592));
#12604=CARTESIAN_POINT('Ctrl Pts',(-71.8391803616628,98.7027402403373,-66.070889639494));
#12605=CARTESIAN_POINT('Origin',(-119.078493020361,109.,-80.7499999999988));
#12606=CARTESIAN_POINT('',(-93.4118265169985,98.3074822374623,-78.0787744031255));
#12607=CARTESIAN_POINT('',(-93.4118265169985,98.3074822374623,-78.0787744031255));
#12608=CARTESIAN_POINT('',(-89.310545785853,100.004330985067,-77.4236234448516));
#12609=CARTESIAN_POINT('Ctrl Pts',(-89.3105457858516,100.004330985068,-77.4236234448524));
#12610=CARTESIAN_POINT('Ctrl Pts',(-89.5906127684196,99.7001003271067,-77.3220467399197));
#12611=CARTESIAN_POINT('Ctrl Pts',(-89.9201573466291,99.432691593161,-77.2594832131444));
#12612=CARTESIAN_POINT('Ctrl Pts',(-90.7270152190322,98.9178350153006,-77.2137926604239));
#12613=CARTESIAN_POINT('Ctrl Pts',(-91.275429932033,98.6785063270153,-77.2683334201939));
#12614=CARTESIAN_POINT('Ctrl Pts',(-92.3773154492341,98.3741443355135,-77.5617079439358));
#12615=CARTESIAN_POINT('Ctrl Pts',(-92.930279409063,98.3074822374625,-77.8007530507317));
#12616=CARTESIAN_POINT('Ctrl Pts',(-93.4118265169985,98.3074822374625,-78.0787744031257));
#12617=CARTESIAN_POINT('',(-91.4118265169984,105.235685467738,-81.5428760182629));
#12618=CARTESIAN_POINT('Ctrl Pts',(-91.4118265169984,105.235685467738,-81.5428760182628));
#12619=CARTESIAN_POINT('Ctrl Pts',(-90.930279409063,105.235685467738,-81.2648546658689));
#12620=CARTESIAN_POINT('Ctrl Pts',(-90.4235466956197,105.142197830515,-80.9457346914359));
#12621=CARTESIAN_POINT('Ctrl Pts',(-89.5276720287663,104.732917302591,-80.2955389079813));
#12622=CARTESIAN_POINT('Ctrl Pts',(-89.1396330959697,104.416687991642,-79.9632191485941));
#12623=CARTESIAN_POINT('Ctrl Pts',(-88.6191933845126,103.711566927935,-79.3777677293152));
#12624=CARTESIAN_POINT('Ctrl Pts',(-88.4360002798934,103.294551166156,-79.0871156461153));
#12625=CARTESIAN_POINT('Ctrl Pts',(-88.2882811646739,102.403958803926,-78.5394916564604));
#12626=CARTESIAN_POINT('Ctrl Pts',(-88.3237355082,101.931198710495,-78.281198278488));
#12627=CARTESIAN_POINT('Ctrl Pts',(-88.5726881997782,101.068801289506,-77.8499995679938));
#12628=CARTESIAN_POINT('Ctrl Pts',(-88.8022989313345,100.623349028228,-77.6491867686112));
#12629=CARTESIAN_POINT('Ctrl Pts',(-89.1799219644913,100.151183250598,-77.4741046930827));
#12630=CARTESIAN_POINT('Ctrl Pts',(-89.2438824969059,100.076745862652,-77.4478013653234));
#12631=CARTESIAN_POINT('Ctrl Pts',(-89.3105457858516,100.004330985068,-77.4236234448524));
#12632=CARTESIAN_POINT('',(-91.4118265169984,105.235685467738,-81.5428760182629));
#12633=CARTESIAN_POINT('Ctrl Pts',(-81.8660249138711,98.3074822374626,-71.4128027395504));
#12634=CARTESIAN_POINT('Ctrl Pts',(-82.3237270253547,98.3074822374626,-71.6770571768241));
#12635=CARTESIAN_POINT('Ctrl Pts',(-82.7726916110599,98.3818254132719,-72.0253258196487));
#12636=CARTESIAN_POINT('Ctrl Pts',(-83.5294587228727,98.6836749369366,-72.8018086256385));
#12637=CARTESIAN_POINT('Ctrl Pts',(-83.8381825657519,98.9117809702808,-73.2288909422442));
#12638=CARTESIAN_POINT('Ctrl Pts',(-84.2642108337661,99.4513482675956,-74.0139591549906));
#12639=CARTESIAN_POINT('Ctrl Pts',(-84.4147303979509,99.7982897132532,-74.427397105883));
#12640=CARTESIAN_POINT('Ctrl Pts',(-84.5187012892031,100.598975519632,-75.1573598769691));
#12641=CARTESIAN_POINT('Ctrl Pts',(-84.4719272936971,101.053974393027,-75.4725395573331));
#12642=CARTESIAN_POINT('Ctrl Pts',(-84.2144142894456,101.946025606974,-75.9185651643065));
#12643=CARTESIAN_POINT('Ctrl Pts',(-83.9900828414982,102.430163538118,-76.072953886212));
#12644=CARTESIAN_POINT('Ctrl Pts',(-83.3943596113716,103.332957803082,-76.1947311507971));
#12645=CARTESIAN_POINT('Ctrl Pts',(-83.022912997837,103.751330105905,-76.1639500741449));
#12646=CARTESIAN_POINT('Ctrl Pts',(-82.2465265160762,104.425439262707,-75.9857200884568));
#12647=CARTESIAN_POINT('Ctrl Pts',(-81.7851543098186,104.72612267149,-75.8230324929145));
#12648=CARTESIAN_POINT('Ctrl Pts',(-80.8241649502783,105.131719766025,-75.4002729960248));
#12649=CARTESIAN_POINT('Ctrl Pts',(-80.3237270253549,105.235685467738,-75.1411587919613));
#12650=CARTESIAN_POINT('Ctrl Pts',(-79.8660249138712,105.235685467738,-74.8769043546876));
#12651=CARTESIAN_POINT('Origin',(-119.078493020361,109.,-80.7499999999988));
#12652=CARTESIAN_POINT('',(-104.90435628947,98.3074822374622,-84.7139895609318));
#12653=CARTESIAN_POINT('',(-104.90435628947,98.3074822374623,-84.7139895609318));
#12654=CARTESIAN_POINT('',(-99.9488699419194,100.228885141061,-83.7562504402684));
#12655=CARTESIAN_POINT('Ctrl Pts',(-99.9488699419193,100.228885141061,-83.7562504402685));
#12656=CARTESIAN_POINT('Ctrl Pts',(-100.269274778488,99.8589135037763,-83.6332987009061));
#12657=CARTESIAN_POINT('Ctrl Pts',(-100.672060551272,99.5388009858237,-83.5687616798079));
#12658=CARTESIAN_POINT('Ctrl Pts',(-101.656557156406,98.9446450743508,-83.5546921849167));
#12659=CARTESIAN_POINT('Ctrl Pts',(-102.323796076877,98.6892023001508,-83.659021954752));
#12660=CARTESIAN_POINT('Ctrl Pts',(-103.656688844209,98.3714816818226,-84.070990296531));
#12661=CARTESIAN_POINT('Ctrl Pts',(-104.322168303632,98.3074822374624,-84.3778631705889));
#12662=CARTESIAN_POINT('Ctrl Pts',(-104.90435628947,98.3074822374624,-84.7139895609318));
#12663=CARTESIAN_POINT('',(-102.90435628947,105.235685467738,-88.1780911760691));
#12664=CARTESIAN_POINT('Ctrl Pts',(-102.90435628947,105.235685467738,-88.178091176069));
#12665=CARTESIAN_POINT('Ctrl Pts',(-102.322168303632,105.235685467738,-87.8419647857261));
#12666=CARTESIAN_POINT('Ctrl Pts',(-101.701146422792,105.145679342323,-87.4580891267805));
#12667=CARTESIAN_POINT('Ctrl Pts',(-100.583248552382,104.718635790978,-86.6737387001651));
#12668=CARTESIAN_POINT('Ctrl Pts',(-100.087436405043,104.380238803494,-86.2724890494876));
#12669=CARTESIAN_POINT('Ctrl Pts',(-99.4797157079115,103.63823946452,-85.6153691751923));
#12670=CARTESIAN_POINT('Ctrl Pts',(-99.2762414496599,103.243002384244,-85.320427254354));
#12671=CARTESIAN_POINT('Ctrl Pts',(-99.0952115751188,102.385815407921,-84.7678773474479));
#12672=CARTESIAN_POINT('Ctrl Pts',(-99.1179825761209,101.924673720388,-84.5089097354468));
#12673=CARTESIAN_POINT('Ctrl Pts',(-99.3631680629044,101.075326279613,-84.0842360150593));
#12674=CARTESIAN_POINT('Ctrl Pts',(-99.5989917777891,100.640669594177,-83.8953044405758));
#12675=CARTESIAN_POINT('Ctrl Pts',(-99.9319639746297,100.248502859387,-83.7627974003584));
#12676=CARTESIAN_POINT('Ctrl Pts',(-99.940389585881,100.238677412744,-83.7595046811735));
#12677=CARTESIAN_POINT('Ctrl Pts',(-99.9488699419193,100.228885141061,-83.7562504402685));
#12678=CARTESIAN_POINT('',(-102.90435628947,105.235685467738,-88.1780911760691));
#12679=CARTESIAN_POINT('Ctrl Pts',(-93.4118265169985,98.3074822374625,-78.0787744031257));
#12680=CARTESIAN_POINT('Ctrl Pts',(-93.9211136281798,98.3074822374625,-78.372811453861));
#12681=CARTESIAN_POINT('Ctrl Pts',(-94.4293110479316,98.3809411378057,-78.7542137874603));
#12682=CARTESIAN_POINT('Ctrl Pts',(-95.3131003585774,98.6801492903014,-79.6011997737382));
#12683=CARTESIAN_POINT('Ctrl Pts',(-95.68953602647,98.9062732240902,-80.0657700699796));
#12684=CARTESIAN_POINT('Ctrl Pts',(-96.2180755930993,99.439773757549,-80.9039616912801));
#12685=CARTESIAN_POINT('Ctrl Pts',(-96.4211158671793,99.7760817327783,-81.3392544545395));
#12686=CARTESIAN_POINT('Ctrl Pts',(-96.603988459357,100.572512615503,-82.1140272198499));
#12687=CARTESIAN_POINT('Ctrl Pts',(-96.5825452086925,101.034655609006,-82.4517288812605));
#12688=CARTESIAN_POINT('Ctrl Pts',(-96.3138784992858,101.965344390996,-82.9170732722552));
#12689=CARTESIAN_POINT('Ctrl Pts',(-96.0594130029196,102.458977333713,-83.0572595789545));
#12690=CARTESIAN_POINT('Ctrl Pts',(-95.3867915721352,103.359086193817,-83.1307566850585));
#12691=CARTESIAN_POINT('Ctrl Pts',(-94.9692620595266,103.765790736204,-83.0669701806072));
#12692=CARTESIAN_POINT('Ctrl Pts',(-94.0943036219507,104.432320373106,-82.8287936444868));
#12693=CARTESIAN_POINT('Ctrl Pts',(-93.5664254574151,104.730808636538,-82.6265294468561));
#12694=CARTESIAN_POINT('Ctrl Pts',(-92.4801710348681,105.132960205189,-82.130223321151));
#12695=CARTESIAN_POINT('Ctrl Pts',(-91.9211136281798,105.235685467738,-81.8369130689982));
#12696=CARTESIAN_POINT('Ctrl Pts',(-91.4118265169984,105.235685467738,-81.5428760182629));
#12697=CARTESIAN_POINT('Origin',(-119.078493020361,109.,-80.7499999999988));
#12698=CARTESIAN_POINT('',(-106.270002469182,105.235685467738,-90.1212479039226));
#12699=CARTESIAN_POINT('',(-106.270002469182,105.235685467738,-90.1212479039226));
#12700=CARTESIAN_POINT('Ctrl Pts',(-104.90435628947,98.3074822374624,-84.7139895609318));
#12701=CARTESIAN_POINT('Ctrl Pts',(-105.520546937821,98.3074822374624,-85.0697473976293));
#12702=CARTESIAN_POINT('Ctrl Pts',(-106.150726410955,98.3786464989181,-85.5188532090103));
#12703=CARTESIAN_POINT('Ctrl Pts',(-107.289220969567,98.6734920739597,-86.5082604731963));
#12704=CARTESIAN_POINT('Ctrl Pts',(-107.798461931632,98.8969623992174,-87.0475589280851));
#12705=CARTESIAN_POINT('Ctrl Pts',(-108.520316145588,99.4223913020677,-87.9892961628252));
#12706=CARTESIAN_POINT('Ctrl Pts',(-108.815648667087,99.7399146036544,-88.4622960553437));
#12707=CARTESIAN_POINT('Ctrl Pts',(-109.06520359177,100.328003547478,-89.1041494241911));
#12708=CARTESIAN_POINT('Ctrl Pts',(-109.116864532686,100.542611823444,-89.3070609778502));
#12709=CARTESIAN_POINT('Ctrl Pts',(-109.140178467765,101.001678002652,-89.6682684715672));
#12710=CARTESIAN_POINT('Ctrl Pts',(-109.111806983136,101.246175947599,-89.8265150985448));
#12711=CARTESIAN_POINT('Ctrl Pts',(-108.965261598155,101.753824052402,-90.080339150946));
#12712=CARTESIAN_POINT('Ctrl Pts',(-108.849954531701,102.007043208325,-90.1709510744033));
#12713=CARTESIAN_POINT('Ctrl Pts',(-108.552569635501,102.497386688197,-90.2844484102263));
#12714=CARTESIAN_POINT('Ctrl Pts',(-108.370506562727,102.734504647816,-90.3073999743598));
#12715=CARTESIAN_POINT('Ctrl Pts',(-107.75853069038,103.401878694155,-90.2932781005938));
#12716=CARTESIAN_POINT('Ctrl Pts',(-107.260215630608,103.787507531247,-90.1718542774143));
#12717=CARTESIAN_POINT('Ctrl Pts',(-106.197183712277,104.44395286517,-89.8210541610607));
#12718=CARTESIAN_POINT('Ctrl Pts',(-105.538070840598,104.739654064067,-89.5413414682492));
#12719=CARTESIAN_POINT('Ctrl Pts',(-104.200003266355,105.136149694813,-88.8976048069571));
#12720=CARTESIAN_POINT('Ctrl Pts',(-103.520546937821,105.235685467738,-88.5338490127664));
#12721=CARTESIAN_POINT('Ctrl Pts',(-102.90435628947,105.235685467738,-88.178091176069));
#12722=CARTESIAN_POINT('',(-108.270002469182,98.3074822374624,-86.6571462887851));
#12723=CARTESIAN_POINT('',(-108.270002469182,98.3074822374623,-86.6571462887851));
#12724=CARTESIAN_POINT('Ctrl Pts',(-106.270002469182,105.235685467738,-90.1212479039226));
#12725=CARTESIAN_POINT('Ctrl Pts',(-106.398364251285,105.235685467738,-90.1953576133737));
#12726=CARTESIAN_POINT('Ctrl Pts',(-106.527960736738,105.218918283964,-90.2651932010029));
#12727=CARTESIAN_POINT('Ctrl Pts',(-106.847366026658,105.139174343852,-90.425397613589));
#12728=CARTESIAN_POINT('Ctrl Pts',(-107.033287150629,105.059113530962,-90.5082215504996));
#12729=CARTESIAN_POINT('Ctrl Pts',(-107.487244640969,104.791037335221,-90.6836023495469));
#12730=CARTESIAN_POINT('Ctrl Pts',(-107.742055343965,104.569575136487,-90.7553778221103));
#12731=CARTESIAN_POINT('Ctrl Pts',(-108.312044999287,103.952474510198,-90.8506321914898));
#12732=CARTESIAN_POINT('Ctrl Pts',(-108.601687275107,103.516179693072,-90.83222067748));
#12733=CARTESIAN_POINT('Ctrl Pts',(-109.016285784176,102.748005272445,-90.6902990309755));
#12734=CARTESIAN_POINT('Ctrl Pts',(-109.166799177582,102.411600006565,-90.5937735724328));
#12735=CARTESIAN_POINT('Ctrl Pts',(-109.364309285276,101.886060973467,-90.3923049613581));
#12736=CARTESIAN_POINT('Ctrl Pts',(-109.428881856401,101.691891969437,-90.3067091143765));
#12737=CARTESIAN_POINT('Ctrl Pts',(-109.539343060738,101.309363471567,-90.1154913997023));
#12738=CARTESIAN_POINT('Ctrl Pts',(-109.58547134865,101.12019828098,-90.0094768684831));
#12739=CARTESIAN_POINT('Ctrl Pts',(-109.683806016576,100.621556930253,-89.6991065970049));
#12740=CARTESIAN_POINT('Ctrl Pts',(-109.718746169311,100.316400657043,-89.4751827475122));
#12741=CARTESIAN_POINT('Ctrl Pts',(-109.719931149862,99.6457292128168,-88.8981274115455));
#12742=CARTESIAN_POINT('Ctrl Pts',(-109.659507933391,99.2872907854466,-88.5188240602725));
#12743=CARTESIAN_POINT('Ctrl Pts',(-109.407078555524,98.8025861049536,-87.8721136642323));
#12744=CARTESIAN_POINT('Ctrl Pts',(-109.264504916411,98.6353091816041,-87.6059682053067));
#12745=CARTESIAN_POINT('Ctrl Pts',(-108.94540320403,98.4361359224893,-87.1969059803222));
#12746=CARTESIAN_POINT('Ctrl Pts',(-108.799409958408,98.3776732407719,-87.0447641078801));
#12747=CARTESIAN_POINT('Ctrl Pts',(-108.519683286228,98.3196123402596,-86.8155806823361));
#12748=CARTESIAN_POINT('Ctrl Pts',(-108.39839753492,98.3074822374624,-86.7312752145517));
#12749=CARTESIAN_POINT('Ctrl Pts',(-108.270002469182,98.3074822374624,-86.6571462887851));
#12750=CARTESIAN_POINT('Origin',(-119.078493020361,109.,-80.7499999999988));
#12751=CARTESIAN_POINT('',(-85.1260169266464,123.456832294801,-65.7663309411545));
#12752=CARTESIAN_POINT('',(-73.5607164801933,123.456832294801,-59.0891016151359));
#12753=CARTESIAN_POINT('',(-85.1260169266463,123.456832294801,-65.7663309411548));
#12754=CARTESIAN_POINT('',(-83.1162922298706,123.872941359692,-62.2368404208554));
#12755=CARTESIAN_POINT('Ctrl Pts',(-83.1162922298706,123.872941359692,-62.2368404208554));
#12756=CARTESIAN_POINT('Ctrl Pts',(-83.1062743831766,123.829770440363,-62.6116107413721));
#12757=CARTESIAN_POINT('Ctrl Pts',(-83.1509026868771,123.7792071983,-62.9828538443025));
#12758=CARTESIAN_POINT('Ctrl Pts',(-83.3664532434541,123.66173721786,-63.8135927138417));
#12759=CARTESIAN_POINT('Ctrl Pts',(-83.6030554954123,123.587986446344,-64.3071289633042));
#12760=CARTESIAN_POINT('Ctrl Pts',(-84.2623538476765,123.484750532966,-65.1560397594667));
#12761=CARTESIAN_POINT('Ctrl Pts',(-84.6849506657898,123.456832294801,-65.5116812167184));
#12762=CARTESIAN_POINT('Ctrl Pts',(-85.1260169266465,123.456832294801,-65.7663309411545));
#12763=CARTESIAN_POINT('',(-89.1260169266464,123.456832294801,-58.8381277108788));
#12764=CARTESIAN_POINT('Ctrl Pts',(-89.1260169266463,123.456832294801,-58.8381277108789));
#12765=CARTESIAN_POINT('Ctrl Pts',(-88.6849506657896,123.456832294801,-58.5834779864428));
#12766=CARTESIAN_POINT('Ctrl Pts',(-88.165657720114,123.484750532965,-58.395319135024));
#12767=CARTESIAN_POINT('Ctrl Pts',(-87.1008302289584,123.587986446343,-58.2488054113713));
#12768=CARTESIAN_POINT('Ctrl Pts',(-86.5551141732562,123.66173721786,-58.2906699753141));
#12769=CARTESIAN_POINT('Ctrl Pts',(-85.5888213740156,123.798956955934,-58.5578170932871));
#12770=CARTESIAN_POINT('Ctrl Pts',(-85.1044718647574,123.871021105468,-58.7975024013151));
#12771=CARTESIAN_POINT('Ctrl Pts',(-84.2687404142013,123.972199967385,-59.4532843052146));
#12772=CARTESIAN_POINT('Ctrl Pts',(-83.9170521365101,124.,-59.8691926348772));
#12773=CARTESIAN_POINT('Ctrl Pts',(-83.4144629487118,124.,-60.7397026434787));
#12774=CARTESIAN_POINT('Ctrl Pts',(-83.2301199084241,123.972199967385,-61.2522277910038));
#12775=CARTESIAN_POINT('Ctrl Pts',(-83.1333491468145,123.906950854201,-61.9304287037879));
#12776=CARTESIAN_POINT('Ctrl Pts',(-83.120379607442,123.890555509,-62.0839305341979));
#12777=CARTESIAN_POINT('Ctrl Pts',(-83.1162922298706,123.872941359692,-62.2368404208553));
#12778=CARTESIAN_POINT('',(-77.5607164801934,123.456832294801,-52.1608983848601));
#12779=CARTESIAN_POINT('',(-89.1260169266463,123.456832294801,-58.8381277108789));
#12780=CARTESIAN_POINT('',(-75.5607164801928,123.594519519327,-59.6249999999981));
#12781=CARTESIAN_POINT('Ctrl Pts',(-75.5607164801923,123.594519519327,-59.6249999999981));
#12782=CARTESIAN_POINT('Ctrl Pts',(-75.9177670555452,123.636893626714,-59.6249999999981));
#12783=CARTESIAN_POINT('Ctrl Pts',(-76.270167318939,123.685122421852,-59.576007942327));
#12784=CARTESIAN_POINT('Ctrl Pts',(-77.0792037993761,123.798839176147,-59.3592272707466));
#12785=CARTESIAN_POINT('Ctrl Pts',(-77.5695548504124,123.870716769224,-59.1248365924091));
#12786=CARTESIAN_POINT('Ctrl Pts',(-78.4161592503826,123.971970182233,-58.476444301003));
#12787=CARTESIAN_POINT('Ctrl Pts',(-78.7723947994248,124.,-58.0622099735219));
#12788=CARTESIAN_POINT('Ctrl Pts',(-79.2772413912376,124.,-57.1877900264742));
#12789=CARTESIAN_POINT('Ctrl Pts',(-79.4578610674346,123.971970182233,-56.672163827532));
#12790=CARTESIAN_POINT('Ctrl Pts',(-79.5960830634252,123.870716769223,-55.6147867644991));
#12791=CARTESIAN_POINT('Ctrl Pts',(-79.5538958197575,123.798839176147,-55.0729349583605));
#12792=CARTESIAN_POINT('Ctrl Pts',(-79.2949201129009,123.662988149345,-54.1064244624455));
#12793=CARTESIAN_POINT('Ctrl Pts',(-79.0605274269875,123.589960152211,-53.6161302759907));
#12794=CARTESIAN_POINT('Ctrl Pts',(-78.4121993371972,123.486046379795,-52.7696054406997));
#12795=CARTESIAN_POINT('Ctrl Pts',(-77.9980062737959,123.456832294801,-52.4133677649104));
#12796=CARTESIAN_POINT('Ctrl Pts',(-77.5607164801933,123.456832294801,-52.1608983848601));
#12797=CARTESIAN_POINT('Ctrl Pts',(-73.5607164801933,123.456832294801,-59.0891016151359));
#12798=CARTESIAN_POINT('Ctrl Pts',(-73.9980062737958,123.456832294801,-59.3415709951862));
#12799=CARTESIAN_POINT('Ctrl Pts',(-74.5136136825151,123.486046379796,-59.5221538722684));
#12800=CARTESIAN_POINT('Ctrl Pts',(-75.214498480876,123.554932441228,-59.6137729046024));
#12801=CARTESIAN_POINT('Ctrl Pts',(-75.3881510574346,123.57403977147,-59.6249999999981));
#12802=CARTESIAN_POINT('Ctrl Pts',(-75.5607164801923,123.594519519327,-59.6249999999981));
#12803=CARTESIAN_POINT('Origin',(-119.078493020361,109.,-80.7499999999988));
#12804=CARTESIAN_POINT('',(-96.6718185297735,123.456832294801,-72.4323026047302));
#12805=CARTESIAN_POINT('',(-96.6718185297736,123.456832294801,-72.4323026047302));
#12806=CARTESIAN_POINT('',(-94.4177421038261,123.892951352905,-68.5776999378933));
#12807=CARTESIAN_POINT('Ctrl Pts',(-94.4177421038264,123.892951352906,-68.5776999378912));
#12808=CARTESIAN_POINT('Ctrl Pts',(-94.3950722235507,123.847611592354,-69.0004788607279));
#12809=CARTESIAN_POINT('Ctrl Pts',(-94.4446100038828,123.791696326041,-69.4229013343407));
#12810=CARTESIAN_POINT('Ctrl Pts',(-94.6962798517419,123.665476993059,-70.3388246478844));
#12811=CARTESIAN_POINT('Ctrl Pts',(-94.9708319480395,123.588576370395,-70.867709374078));
#12812=CARTESIAN_POINT('Ctrl Pts',(-95.7182701307845,123.483657833973,-71.7750046897054));
#12813=CARTESIAN_POINT('Ctrl Pts',(-96.1902714218383,123.456832294801,-72.154281252336));
#12814=CARTESIAN_POINT('Ctrl Pts',(-96.6718185297737,123.456832294801,-72.43230260473));
#12815=CARTESIAN_POINT('',(-100.671818529773,123.456832294801,-65.5040993744542));
#12816=CARTESIAN_POINT('Ctrl Pts',(-100.671818529773,123.456832294801,-65.5040993744543));
#12817=CARTESIAN_POINT('Ctrl Pts',(-100.198890562852,123.456832294801,-65.2310542854448));
#12818=CARTESIAN_POINT('Ctrl Pts',(-99.6449352638787,123.482663841571,-65.0141879033647));
#12819=CARTESIAN_POINT('Ctrl Pts',(-98.5058533293481,123.584301615867,-64.8160574918001));
#12820=CARTESIAN_POINT('Ctrl Pts',(-97.9204236427471,123.659016564532,-64.8359793331119));
#12821=CARTESIAN_POINT('Ctrl Pts',(-96.9056954794152,123.797787553474,-65.0846768377439));
#12822=CARTESIAN_POINT('Ctrl Pts',(-96.4098673945079,123.869713255231,-65.3135356756117));
#12823=CARTESIAN_POINT('Ctrl Pts',(-95.5559638106463,123.971567821815,-65.9593477666097));
#12824=CARTESIAN_POINT('Ctrl Pts',(-95.1973252908835,124.,-66.3757915444938));
#12825=CARTESIAN_POINT('Ctrl Pts',(-94.6944496907949,124.,-67.2467976337339));
#12826=CARTESIAN_POINT('Ctrl Pts',(-94.5146381715445,123.972692167848,-67.755124974498));
#12827=CARTESIAN_POINT('Ctrl Pts',(-94.4324796442889,123.913947930132,-68.376407921987));
#12828=CARTESIAN_POINT('Ctrl Pts',(-94.4231381300388,123.903743405331,-68.4770674633497));
#12829=CARTESIAN_POINT('Ctrl Pts',(-94.4177421038264,123.892951352906,-68.5776999378912));
#12830=CARTESIAN_POINT('',(-100.671818529773,123.456832294801,-65.5040993744543));
#12831=CARTESIAN_POINT('Ctrl Pts',(-85.1260169266465,123.456832294801,-65.7663309411545));
#12832=CARTESIAN_POINT('Ctrl Pts',(-85.5837190381301,123.456832294801,-66.0305853784282));
#12833=CARTESIAN_POINT('Ctrl Pts',(-86.122720562641,123.486454820705,-66.2229054686833));
#12834=CARTESIAN_POINT('Ctrl Pts',(-87.2307450620227,123.590202391576,-66.3909926328699));
#12835=CARTESIAN_POINT('Ctrl Pts',(-87.7998683754043,123.662779767014,-66.3670498363015));
#12836=CARTESIAN_POINT('Ctrl Pts',(-88.8096922981326,123.797321626501,-66.140954313845));
#12837=CARTESIAN_POINT('Ctrl Pts',(-89.3225329048017,123.868752483667,-65.9268338105032));
#12838=CARTESIAN_POINT('Ctrl Pts',(-90.208346563904,123.970860942253,-65.3026051841426));
#12839=CARTESIAN_POINT('Ctrl Pts',(-90.5808483157038,124.,-64.8915779677916));
#12840=CARTESIAN_POINT('Ctrl Pts',(-91.095874324207,124.,-63.9995267538447));
#12841=CARTESIAN_POINT('Ctrl Pts',(-91.2655834593138,123.970860942253,-63.4714171656563));
#12842=CARTESIAN_POINT('Ctrl Pts',(-91.3632744779603,123.868752483666,-62.3921657206742));
#12843=CARTESIAN_POINT('Ctrl Pts',(-91.2922879699909,123.797321626501,-61.8409724755356));
#12844=CARTESIAN_POINT('Ctrl Pts',(-90.9831804747559,123.662779767014,-60.8533915438754));
#12845=CARTESIAN_POINT('Ctrl Pts',(-90.7193538881309,123.590202391575,-60.3485448983168));
#12846=CARTESIAN_POINT('Ctrl Pts',(-90.0197738842044,123.486454820704,-59.47301111593));
#12847=CARTESIAN_POINT('Ctrl Pts',(-89.5837190381299,123.456832294801,-59.1023821481526));
#12848=CARTESIAN_POINT('Ctrl Pts',(-89.1260169266463,123.456832294801,-58.8381277108788));
#12849=CARTESIAN_POINT('Origin',(-119.078493020361,109.,-80.7499999999988));
#12850=CARTESIAN_POINT('',(-108.164348302245,123.456832294801,-79.0675177625366));
#12851=CARTESIAN_POINT('',(-108.164348302245,123.456832294801,-79.0675177625365));
#12852=CARTESIAN_POINT('',(-105.277091391218,123.923615035047,-74.5275001761057));
#12853=CARTESIAN_POINT('Ctrl Pts',(-105.277091391218,123.923615035047,-74.5275001761056));
#12854=CARTESIAN_POINT('Ctrl Pts',(-105.275365738248,123.921622422635,-74.5492158639596));
#12855=CARTESIAN_POINT('Ctrl Pts',(-105.273837242761,123.919598892701,-74.5709499461767));
#12856=CARTESIAN_POINT('Ctrl Pts',(-105.238853605271,123.865658954398,-75.1423248070353));
#12857=CARTESIAN_POINT('Ctrl Pts',(-105.33860750079,123.794453706366,-75.701175262549));
#12858=CARTESIAN_POINT('Ctrl Pts',(-105.746737061739,123.654133883405,-76.7806745481755));
#12859=CARTESIAN_POINT('Ctrl Pts',(-106.120272716169,123.5787523934,-77.3509626000236));
#12860=CARTESIAN_POINT('Ctrl Pts',(-107.054281271328,123.479989785222,-78.3346823431572));
#12861=CARTESIAN_POINT('Ctrl Pts',(-107.613395871184,123.456832294801,-78.7494252281526));
#12862=CARTESIAN_POINT('Ctrl Pts',(-108.164348302246,123.456832294801,-79.0675177625365));
#12863=CARTESIAN_POINT('',(-112.164348302245,123.456832294801,-72.1393145322606));
#12864=CARTESIAN_POINT('Ctrl Pts',(-112.164348302245,123.456832294801,-72.1393145322606));
#12865=CARTESIAN_POINT('Ctrl Pts',(-111.613395871184,123.456832294801,-71.8212219978767));
#12866=CARTESIAN_POINT('Ctrl Pts',(-110.974660696811,123.479989785221,-71.5443859932717));
#12867=CARTESIAN_POINT('Ctrl Pts',(-109.655730131473,123.578752393399,-71.2273707287195));
#12868=CARTESIAN_POINT('Ctrl Pts',(-108.975078363883,123.654133883405,-71.1890233886878));
#12869=CARTESIAN_POINT('Ctrl Pts',(-107.836139778689,123.794453706366,-71.3753224636836));
#12870=CARTESIAN_POINT('Ctrl Pts',(-107.302284139538,123.865658954397,-71.5683582837951));
#12871=CARTESIAN_POINT('Ctrl Pts',(-106.383953947217,123.96943271423,-72.1762726463728));
#12872=CARTESIAN_POINT('Ctrl Pts',(-105.998960269092,124.,-72.5907067654734));
#12873=CARTESIAN_POINT('Ctrl Pts',(-105.482985495051,124.,-73.4844012895352));
#12874=CARTESIAN_POINT('Ctrl Pts',(-105.318978111356,123.971981653342,-74.0003959692113));
#12875=CARTESIAN_POINT('Ctrl Pts',(-105.277091391218,123.923615035047,-74.5275001761056));
#12876=CARTESIAN_POINT('',(-112.164348302245,123.456832294801,-72.1393145322605));
#12877=CARTESIAN_POINT('Ctrl Pts',(-96.6718185297737,123.456832294801,-72.43230260473));
#12878=CARTESIAN_POINT('Ctrl Pts',(-97.2080109095617,123.456832294801,-72.741873419538));
#12879=CARTESIAN_POINT('Ctrl Pts',(-97.8378331599511,123.489300624785,-72.9756291788421));
#12880=CARTESIAN_POINT('Ctrl Pts',(-99.1346770015159,123.601479985038,-73.210267194341));
#12881=CARTESIAN_POINT('Ctrl Pts',(-99.801733680399,123.679673134231,-73.2116784585455));
#12882=CARTESIAN_POINT('Ctrl Pts',(-100.899904621245,123.812998388381,-73.0077930813484));
#12883=CARTESIAN_POINT('Ctrl Pts',(-101.417162434113,123.877803175384,-72.8258148556167));
#12884=CARTESIAN_POINT('Ctrl Pts',(-102.313026843884,123.972069837582,-72.2590940486296));
#12885=CARTESIAN_POINT('Ctrl Pts',(-102.69054002654,124.,-71.8723715243807));
#12886=CARTESIAN_POINT('Ctrl Pts',(-103.196264738206,124.,-70.9964306291323));
#12887=CARTESIAN_POINT('Ctrl Pts',(-103.342419677093,123.972069837582,-70.4761333605637));
#12888=CARTESIAN_POINT('Ctrl Pts',(-103.385282087912,123.877803175384,-69.4169316198625));
#12889=CARTESIAN_POINT('Ctrl Pts',(-103.284250947897,123.812998388381,-68.8779841007473));
#12890=CARTESIAN_POINT('Ctrl Pts',(-102.911735393587,123.67967313423,-67.8249974796778));
#12891=CARTESIAN_POINT('Ctrl Pts',(-102.576984863492,123.601479985038,-67.2480150821033));
#12892=CARTESIAN_POINT('Ctrl Pts',(-101.725360460594,123.489300624784,-66.2422343783163));
#12893=CARTESIAN_POINT('Ctrl Pts',(-101.208010909561,123.456832294801,-65.8136701892623));
#12894=CARTESIAN_POINT('Ctrl Pts',(-100.671818529773,123.456832294801,-65.5040993744543));
#12895=CARTESIAN_POINT('Origin',(-119.078493020361,109.,-80.7499999999988));
#12896=CARTESIAN_POINT('',(-115.529994481957,123.456832294801,-74.0824712601142));
#12897=CARTESIAN_POINT('',(-115.529994481957,123.456832294801,-74.082471260114));
#12898=CARTESIAN_POINT('Ctrl Pts',(-108.164348302246,123.456832294801,-79.0675177625365));
#12899=CARTESIAN_POINT('Ctrl Pts',(-108.844463055017,123.456832294801,-79.4601821981288));
#12900=CARTESIAN_POINT('Ctrl Pts',(-109.637912977074,123.491441900927,-79.7804741154724));
#12901=CARTESIAN_POINT('Ctrl Pts',(-111.275183810088,123.611693066724,-80.170706138189));
#12902=CARTESIAN_POINT('Ctrl Pts',(-112.118571906507,123.696010228407,-80.2428658921871));
#12903=CARTESIAN_POINT('Ctrl Pts',(-113.398550856209,123.828649318389,-80.1045968599479));
#12904=CARTESIAN_POINT('Ctrl Pts',(-113.937605814753,123.885984825864,-79.974373351834));
#12905=CARTESIAN_POINT('Ctrl Pts',(-114.643393821985,123.950735654834,-79.6153146748024));
#12906=CARTESIAN_POINT('Ctrl Pts',(-114.862132214305,123.968740024147,-79.4686771786292));
#12907=CARTESIAN_POINT('Ctrl Pts',(-115.243722739859,123.993392806363,-79.1229603686417));
#12908=CARTESIAN_POINT('Ctrl Pts',(-115.406496999395,124.,-78.9237921724865));
#12909=CARTESIAN_POINT('Ctrl Pts',(-115.660952638663,124.,-78.4830620770019));
#12910=CARTESIAN_POINT('Ctrl Pts',(-115.752050226392,123.993392806363,-78.2425113350836));
#12911=CARTESIAN_POINT('Ctrl Pts',(-115.860654503579,123.968740024147,-77.7391858411162));
#12912=CARTESIAN_POINT('Ctrl Pts',(-115.878277104252,123.950735654834,-77.4764340884979));
#12913=CARTESIAN_POINT('Ctrl Pts',(-115.836337036395,123.885984825864,-76.6856744060329));
#12914=CARTESIAN_POINT('Ctrl Pts',(-115.679586423319,123.828649318388,-76.1537273638406));
#12915=CARTESIAN_POINT('Ctrl Pts',(-115.159341442944,123.696010228406,-74.9760985609694));
#12916=CARTESIAN_POINT('Ctrl Pts',(-114.675155214641,123.611693066724,-74.2817829212208));
#12917=CARTESIAN_POINT('Ctrl Pts',(-113.518568953091,123.491441900926,-73.0589807983134));
#12918=CARTESIAN_POINT('Ctrl Pts',(-112.844463055016,123.456832294801,-72.531978967853));
#12919=CARTESIAN_POINT('Ctrl Pts',(-112.164348302245,123.456832294801,-72.1393145322606));
#12920=CARTESIAN_POINT('',(-111.529994481957,123.456832294801,-81.0106744903897));
#12921=CARTESIAN_POINT('',(-111.529994481957,123.456832294801,-81.0106744903897));
#12922=CARTESIAN_POINT('Ctrl Pts',(-115.529994481957,123.456832294801,-74.0824712601142));
#12923=CARTESIAN_POINT('Ctrl Pts',(-115.65835626406,123.456832294801,-74.1565809695654));
#12924=CARTESIAN_POINT('Ctrl Pts',(-115.77745320865,123.461475653088,-74.2446022954246));
#12925=CARTESIAN_POINT('Ctrl Pts',(-116.046607194207,123.483194384997,-74.4918445203156));
#12926=CARTESIAN_POINT('Ctrl Pts',(-116.181936272838,123.504836535895,-74.6622964502142));
#12927=CARTESIAN_POINT('Ctrl Pts',(-116.463492476953,123.573840873615,-75.1362850362945));
#12928=CARTESIAN_POINT('Ctrl Pts',(-116.573472758241,123.62806730643,-75.4589141577373));
#12929=CARTESIAN_POINT('Ctrl Pts',(-116.724373411066,123.761245635907,-76.2800519723337));
#12930=CARTESIAN_POINT('Ctrl Pts',(-116.704520006728,123.840165624527,-76.7977027010819));
#12931=CARTESIAN_POINT('Ctrl Pts',(-116.53883398008,123.93828517935,-77.6608633532843));
#12932=CARTESIAN_POINT('Ctrl Pts',(-116.424541973442,123.968919507233,-78.0229943017362));
#12933=CARTESIAN_POINT('Ctrl Pts',(-116.189563012637,123.995063180093,-78.5706187310189));
#12934=CARTESIAN_POINT('Ctrl Pts',(-116.090247091074,123.99999005338,-78.7688860801498));
#12935=CARTESIAN_POINT('Ctrl Pts',(-115.86944609645,124.000009911765,-79.1514313247033));
#12936=CARTESIAN_POINT('Ctrl Pts',(-115.74750688821,123.995107474062,-79.3365182359193));
#12937=CARTESIAN_POINT('Ctrl Pts',(-115.391456612351,123.969070285569,-79.8131657732718));
#12938=CARTESIAN_POINT('Ctrl Pts',(-115.135714858818,123.938576005114,-80.0927177542768));
#12939=CARTESIAN_POINT('Ctrl Pts',(-114.471237782264,123.840607113622,-80.6686229218872));
#12940=CARTESIAN_POINT('Ctrl Pts',(-114.031900126614,123.761512834073,-80.9456186309926));
#12941=CARTESIAN_POINT('Ctrl Pts',(-113.24419775823,123.628137504237,-81.2260282504464));
#12942=CARTESIAN_POINT('Ctrl Pts',(-112.909789654842,123.573903068408,-81.292149830288));
#12943=CARTESIAN_POINT('Ctrl Pts',(-112.358412824606,123.504868123884,-81.2853999107625));
#12944=CARTESIAN_POINT('Ctrl Pts',(-112.143032917437,123.483209990156,-81.2534392614886));
#12945=CARTESIAN_POINT('Ctrl Pts',(-111.794203638433,123.461478073366,-81.1439450618975));
#12946=CARTESIAN_POINT('Ctrl Pts',(-111.658389547695,123.456832294801,-81.0848034161563));
#12947=CARTESIAN_POINT('Ctrl Pts',(-111.529994481957,123.456832294801,-81.0106744903897));
#12948=CARTESIAN_POINT('Origin',(-119.078493020361,109.,-80.7499999999988));
#12949=CARTESIAN_POINT('',(-126.564449609913,108.0824948189,-67.7839428436388));
#12950=CARTESIAN_POINT('',(-122.424179917669,122.42480974691,-74.9551003076436));
#12951=CARTESIAN_POINT('Origin',(-119.078493020361,109.,-80.7499999999988));
#12952=CARTESIAN_POINT('',(-77.2010015942,108.0824948189,-39.2839428436393));
#12953=CARTESIAN_POINT('',(-126.564449609913,108.0824948189,-67.7839428436388));
#12954=CARTESIAN_POINT('',(-73.0607319019557,122.42480974691,-46.4551003076441));
#12955=CARTESIAN_POINT('Origin',(-69.7150450046476,109.,-52.2499999999992));
#12956=CARTESIAN_POINT('',(-122.424179917669,122.42480974691,-74.9551003076436));
#12957=CARTESIAN_POINT('Origin',(-69.7150450046476,109.,-52.2499999999992));
#12958=CARTESIAN_POINT('',(-73.7335498795933,101.937180526609,-39.2897453861299));
#12959=CARTESIAN_POINT('',(-70.2694482644555,101.937180526609,-37.2897453861299));
#12960=CARTESIAN_POINT('',(-73.7335498795933,101.937180526609,-39.2897453861299));
#12961=CARTESIAN_POINT('',(-67.366968793295,123.991664350565,-50.3169872981059));
#12962=CARTESIAN_POINT('Origin',(-67.1169687932943,109.,-50.7499999999993));
#12963=CARTESIAN_POINT('',(-63.9028671781572,123.991664350565,-48.3169872981059));
#12964=CARTESIAN_POINT('',(-67.366968793295,123.991664350565,-50.3169872981059));
#12965=CARTESIAN_POINT('Origin',(-63.6528671781565,109.,-48.7499999999993));
#12966=CARTESIAN_POINT('Origin',(-69.7150450046476,109.,-52.2499999999992));
#12967=CARTESIAN_POINT('',(-78.2150450046475,109.,-37.5275681356637));
#12968=CARTESIAN_POINT('Origin',(-69.7150450046476,109.,-52.2499999999992));
#12969=CARTESIAN_POINT('',(-76.9580463854329,108.363035329266,-39.7047536091873));
#12970=CARTESIAN_POINT('',(-76.9580463854329,108.363035329266,-39.7047536091873));
#12971=CARTESIAN_POINT('',(-73.6123594881249,96.7732359445554,-45.4996533015424));
#12972=CARTESIAN_POINT('Origin',(-69.7150450046476,109.,-52.2499999999992));
#12973=CARTESIAN_POINT('',(-73.6123594881249,96.7732359445554,-45.4996533015424));
#12974=CARTESIAN_POINT('',(-65.8177305211704,96.7732359445554,-59.0003466984559));
#12975=CARTESIAN_POINT('',(-65.8177305211704,96.7732359445554,-59.0003466984559));
#12976=CARTESIAN_POINT('',(-62.4720436238624,108.363035329266,-64.7952463908111));
#12977=CARTESIAN_POINT('Origin',(-69.7150450046476,109.,-52.2499999999992));
#12978=CARTESIAN_POINT('',(-62.4720436238624,108.363035329266,-64.7952463908111));
#12979=CARTESIAN_POINT('',(-66.3693581073396,121.863728726179,-58.0448996923544));
#12980=CARTESIAN_POINT('',(-66.3693581073396,121.863728726179,-58.0448996923544));
#12981=CARTESIAN_POINT('',(-73.0607319019557,121.863728726179,-46.4551003076441));
#12982=CARTESIAN_POINT('Origin',(-69.7150450046476,109.,-52.2499999999992));
#12983=CARTESIAN_POINT('',(-73.0607319019557,121.863728726179,-46.4551003076441));
#12984=CARTESIAN_POINT('Origin',(-63.6528671781565,109.,-48.7499999999993));
#12985=CARTESIAN_POINT('',(-72.1528671781564,109.,-34.0275681356638));
#12986=CARTESIAN_POINT('Origin',(-63.6528671781565,109.,-48.7499999999993));
#12987=CARTESIAN_POINT('',(-56.6032733899647,101.437180526611,-60.9602546138697));
#12988=CARTESIAN_POINT('',(-56.6032733899647,101.437180526611,-60.9602546138697));
#12989=CARTESIAN_POINT('',(-56.8532733899647,100.571155122826,-60.5272419119775));
#12990=CARTESIAN_POINT('',(-56.8532733899647,100.571155122826,-60.5272419119775));
#12991=CARTESIAN_POINT('',(-57.2862860918569,101.071155122826,-59.7772419119775));
#12992=CARTESIAN_POINT('',(-70.4524609663477,100.571155122824,-36.9727580880222));
#12993=CARTESIAN_POINT('',(-70.4524609663477,100.571155122824,-36.9727580880222));
#12994=CARTESIAN_POINT('',(-70.7024609663477,101.437180526609,-36.5397453861299));
#12995=CARTESIAN_POINT('',(-70.7024609663477,101.437180526609,-36.53974538613));
#12996=CARTESIAN_POINT('',(-70.2694482644555,101.937180526609,-37.2897453861299));
#12997=CARTESIAN_POINT('',(-63.9028671781572,124.991664350565,-48.3169872981059));
#12998=CARTESIAN_POINT('',(-63.9028671781572,124.991664350565,-48.3169872981059));
#12999=CARTESIAN_POINT('',(-63.4028671781572,124.991664350565,-49.1830127018903));
#13000=CARTESIAN_POINT('',(-63.4028671781572,124.991664350565,-49.1830127018903));
#13001=CARTESIAN_POINT('',(-63.4028671781572,123.991664350565,-49.1830127018903));
#13002=CARTESIAN_POINT('Origin',(-69.7150450046476,109.,-52.2499999999992));
#13003=CARTESIAN_POINT('',(-78.2150450046475,109.,-37.5275681356637));
#13004=CARTESIAN_POINT('Origin',(-67.1169687932943,109.,-50.7499999999993));
#13005=CARTESIAN_POINT('',(-60.3173750051025,100.571155122826,-62.5272419119774));
#13006=CARTESIAN_POINT('',(-60.7503877069946,101.071155122826,-61.7772419119775));
#13007=CARTESIAN_POINT('',(-60.0673750051025,101.437180526611,-62.9602546138697));
#13008=CARTESIAN_POINT('',(-60.3173750051025,100.571155122826,-62.5272419119774));
#13009=CARTESIAN_POINT('',(-60.0673750051025,101.437180526611,-62.9602546138697));
#13010=CARTESIAN_POINT('',(-66.866968793295,124.991664350565,-51.1830127018903));
#13011=CARTESIAN_POINT('',(-66.866968793295,123.991664350565,-51.1830127018903));
#13012=CARTESIAN_POINT('',(-67.366968793295,124.991664350565,-50.3169872981059));
#13013=CARTESIAN_POINT('',(-66.866968793295,124.991664350565,-51.1830127018903));
#13014=CARTESIAN_POINT('',(-67.366968793295,124.991664350565,-50.3169872981059));
#13015=CARTESIAN_POINT('',(-74.1665625814855,101.437180526609,-38.5397453861299));
#13016=CARTESIAN_POINT('',(-73.7335498795933,101.937180526609,-39.2897453861299));
#13017=CARTESIAN_POINT('',(-73.9165625814855,100.571155122824,-38.9727580880221));
#13018=CARTESIAN_POINT('',(-74.1665625814855,101.437180526609,-38.5397453861299));
#13019=CARTESIAN_POINT('',(-73.9165625814855,100.571155122824,-38.9727580880221));
#13020=CARTESIAN_POINT('',(-73.616968793294,109.,-39.4916697508017));
#13021=CARTESIAN_POINT('Origin',(-67.116968793295,109.,-50.7499999999981));
#13022=CARTESIAN_POINT('Origin',(-119.078493020361,109.,-80.7499999999988));
#13023=CARTESIAN_POINT('',(-122.975807503838,96.7732359445554,-73.9996533015419));
#13024=CARTESIAN_POINT('',(-122.975807503838,96.7732359445554,-73.9996533015419));
#13025=CARTESIAN_POINT('',(-126.321494401146,108.363035329266,-68.2047536091869));
#13026=CARTESIAN_POINT('Origin',(-119.078493020361,109.,-80.7499999999988));
#13027=CARTESIAN_POINT('',(-126.564449609913,108.0824948189,-67.7839428436388));
#13028=CARTESIAN_POINT('',(-122.424179917669,121.863728726179,-74.9551003076436));
#13029=CARTESIAN_POINT('',(-122.424179917669,121.863728726179,-74.9551003076436));
#13030=CARTESIAN_POINT('',(-115.732806123053,121.863728726179,-86.5448996923539));
#13031=CARTESIAN_POINT('Origin',(-119.078493020361,109.,-80.7499999999988));
#13032=CARTESIAN_POINT('',(-115.732806123053,122.42480974691,-86.5448996923539));
#13033=CARTESIAN_POINT('',(-111.835491639576,108.363035329266,-93.2952463908107));
#13034=CARTESIAN_POINT('',(-111.835491639576,108.363035329266,-93.2952463908107));
#13035=CARTESIAN_POINT('',(-115.181178536884,96.7732359445553,-87.5003466984555));
#13036=CARTESIAN_POINT('Origin',(-119.078493020361,109.,-80.7499999999988));
#13037=CARTESIAN_POINT('',(-114.938223328117,96.49269543419,-87.9211574640035));
#13038=CARTESIAN_POINT('Origin',(-75.5607164801933,129.,-55.624999999998));
#13039=CARTESIAN_POINT('',(-75.5607164801933,129.,-59.6249999999981));
#13040=CARTESIAN_POINT('Origin',(-75.5607164801933,129.,-55.624999999998));
#13041=CARTESIAN_POINT('',(-75.5607164801933,129.,-59.1249999999981));
#13042=CARTESIAN_POINT('Origin',(-75.5607164801933,129.,-55.624999999998));
#13043=CARTESIAN_POINT('Origin',(-75.5607164801933,-5.00102499999999,-55.624999999998));
#13044=CARTESIAN_POINT('',(-75.5607164801933,-5.00102499999999,-59.6249999999981));
#13045=CARTESIAN_POINT('',(-77.5607164801934,122.937359864766,-52.1608983848606));
#13046=CARTESIAN_POINT('',(-77.5607164801934,122.937359864766,-52.1608983848601));
#13047=CARTESIAN_POINT('',(-73.5607164801933,122.937359864767,-59.0891016151359));
#13048=CARTESIAN_POINT('Ctrl Pts',(-77.5607164801933,122.937359864766,-52.1608983848601));
#13049=CARTESIAN_POINT('Ctrl Pts',(-77.1232537523542,122.937359864766,-51.9083291611818));
#13050=CARTESIAN_POINT('Ctrl Pts',(-76.60754249421,122.967689419789,-51.7277743724565));
#13051=CARTESIAN_POINT('Ctrl Pts',(-75.5502948880754,123.075440885261,-51.5896430799529));
#13052=CARTESIAN_POINT('Ctrl Pts',(-75.008612000326,123.151115999848,-51.6318312278756));
#13053=CARTESIAN_POINT('Ctrl Pts',(-74.0423701006026,123.291794528869,-51.8907349645996));
#13054=CARTESIAN_POINT('Ctrl Pts',(-73.5520995881099,123.366192507349,-52.1250380084307));
#13055=CARTESIAN_POINT('Ctrl Pts',(-72.7054703736856,123.47098799846,-52.7733608760245));
#13056=CARTESIAN_POINT('Ctrl Pts',(-72.3491310307417,123.5,-53.1876291712969));
#13057=CARTESIAN_POINT('Ctrl Pts',(-71.8440986993692,123.5,-54.0623708286991));
#13058=CARTESIAN_POINT('Ctrl Pts',(-71.6635015031528,123.47098799846,-54.5781038996925));
#13059=CARTESIAN_POINT('Ctrl Pts',(-71.5253520371743,123.366192507349,-55.635467740767));
#13060=CARTESIAN_POINT('Ctrl Pts',(-71.5675749052789,123.29179452887,-56.1772059812275));
#13061=CARTESIAN_POINT('Ctrl Pts',(-71.826478642003,123.151115999849,-57.143447880951));
#13062=CARTESIAN_POINT('Ctrl Pts',(-72.060784078038,123.075440885262,-57.6336530964987));
#13063=CARTESIAN_POINT('Ctrl Pts',(-72.709033089471,122.96768941979,-58.4801907352497));
#13064=CARTESIAN_POINT('Ctrl Pts',(-73.1232537523542,122.937359864767,-58.8365323914576));
#13065=CARTESIAN_POINT('Ctrl Pts',(-73.5607164801933,122.937359864767,-59.0891016151359));
#13066=CARTESIAN_POINT('',(-73.5607164801933,122.937359864767,-59.0891016151359));
#13067=CARTESIAN_POINT('Origin',(-88.2037045535141,128.101020514434,-62.924432567491));
#13068=CARTESIAN_POINT('',(-84.3072367627289,129.005199011952,-62.924432567491));
#13069=CARTESIAN_POINT('Origin',(-88.2037045535141,128.101020514434,-62.924432567491));
#13070=CARTESIAN_POINT('',(-84.7942952365771,128.892176699762,-62.9244325674911));
#13071=CARTESIAN_POINT('Origin',(-88.2037045535141,128.101020514434,-62.9244325674911));
#13072=CARTESIAN_POINT('Origin',(-39.9537393796627,-79.8274313593171,-35.0673021859779));
#13073=CARTESIAN_POINT('',(-36.0572715888775,-78.9232528617992,-35.0673021859779));
#13074=CARTESIAN_POINT('Origin',(-100.711351574804,127.535898384862,-70.1457259421618));
#13075=CARTESIAN_POINT('',(-97.1336428108046,129.324752766862,-70.1457259421618));
#13076=CARTESIAN_POINT('Origin',(-100.711351574804,127.535898384862,-70.1457259421618));
#13077=CARTESIAN_POINT('',(-97.5808564063047,129.101145969112,-70.1457259421618));
#13078=CARTESIAN_POINT('Origin',(-100.711351574804,127.535898384862,-70.1457259421618));
#13079=CARTESIAN_POINT('Origin',(24.6400845185815,-123.166973801907,2.2259594296606));
#13080=CARTESIAN_POINT('',(28.2177932825812,-121.378119419907,2.2259594296606));
#13081=CARTESIAN_POINT('Origin',(-113.529994481957,127.343145750508,-77.5465728752519));
#13082=CARTESIAN_POINT('',(-110.506278697883,129.96176043334,-77.5465728752519));
#13083=CARTESIAN_POINT('Origin',(-113.529994481957,127.343145750508,-77.5465728752519));
#13084=CARTESIAN_POINT('',(-110.884243170892,129.634433597986,-77.5465728752519));
#13085=CARTESIAN_POINT('Origin',(-113.529994481957,127.343145750508,-77.5465728752519));
#13086=CARTESIAN_POINT('Origin',(101.486213576105,-120.9361854544,46.5930927272026));
#13087=CARTESIAN_POINT('',(104.509929360179,-118.317570771568,46.5930927272026));
#13088=CARTESIAN_POINT('Origin',(-75.5607164801933,126.,-55.624999999998));
#13089=CARTESIAN_POINT('',(-75.5607164801933,126.,-59.1249999999981));
#13090=CARTESIAN_POINT('Origin',(-75.5607164801933,126.,-55.624999999998));
#13091=CARTESIAN_POINT('',(-75.5607164801933,126.,-58.4249999999981));
#13092=CARTESIAN_POINT('Origin',(-75.5607164801933,126.,-55.624999999998));
#13093=CARTESIAN_POINT('Origin',(-75.5607164801933,126.,-55.624999999998));
#13094=CARTESIAN_POINT('',(-75.5607164801933,126.,-59.1249999999981));
#13095=CARTESIAN_POINT('Origin',(-87.531272949388,125.203243035567,-62.5362039998373));
#13096=CARTESIAN_POINT('',(-84.121863632451,125.994399220895,-62.5362039998373));
#13097=CARTESIAN_POINT('Origin',(-87.531272949388,125.203243035567,-62.5362039998373));
#13098=CARTESIAN_POINT('',(-84.8037454958384,125.836167983829,-62.5362039998373));
#13099=CARTESIAN_POINT('Origin',(-87.531272949388,125.203243035567,-62.5362039998373));
#13100=CARTESIAN_POINT('Origin',(-87.531272949388,125.203243035567,-62.5362039998373));
#13101=CARTESIAN_POINT('',(-84.121863632451,125.994399220895,-62.5362039998373));
#13102=CARTESIAN_POINT('Origin',(-99.4123134691276,124.937822173509,-69.3957259421618));
#13103=CARTESIAN_POINT('',(-96.281818300628,126.503069757759,-69.3957259421618));
#13104=CARTESIAN_POINT('Origin',(-99.4123134691276,124.937822173509,-69.3957259421618));
#13105=CARTESIAN_POINT('',(-96.907917334328,126.190020240909,-69.3957259421618));
#13106=CARTESIAN_POINT('Origin',(-99.4123134691276,124.937822173509,-69.3957259421618));
#13107=CARTESIAN_POINT('Origin',(-99.4123134691276,124.937822173509,-69.3957259421618));
#13108=CARTESIAN_POINT('',(-96.281818300628,126.503069757759,-69.3957259421618));
#13109=CARTESIAN_POINT('Origin',(-147.457758061401,109.,-97.1347763108453));
#13110=CARTESIAN_POINT('',(-122.114391405223,109.,-67.4916697508013));
#13111=CARTESIAN_POINT('Origin',(-115.614391405224,109.,-78.7499999999976));
#13112=CARTESIAN_POINT('',(-153.9577580614,109.,-85.8764460616489));
#13113=CARTESIAN_POINT('',(-117.386134507203,101.605059126311,-67.4270749801284));
#13114=CARTESIAN_POINT('',(-111.565481622863,103.438089404292,-62.8444992851723));
#13115=CARTESIAN_POINT('Ctrl Pts',(-117.386134507204,101.60505912631,-67.4270749801283));
#13116=CARTESIAN_POINT('Ctrl Pts',(-117.384843998764,101.603815224188,-67.4273233385933));
#13117=CARTESIAN_POINT('Ctrl Pts',(-117.383552105126,101.602572260028,-67.4275705183945));
#13118=CARTESIAN_POINT('Ctrl Pts',(-117.105783250958,101.335811456963,-67.4804062339256));
#13119=CARTESIAN_POINT('Ctrl Pts',(-116.763727423833,101.113949509274,-67.4772489203251));
#13120=CARTESIAN_POINT('Ctrl Pts',(-115.970697123411,100.70633252813,-67.3909870285613));
#13121=CARTESIAN_POINT('Ctrl Pts',(-115.446738163493,100.524469125477,-67.2695400568307));
#13122=CARTESIAN_POINT('Ctrl Pts',(-114.405674258994,100.28486436115,-66.9123137382068));
#13123=CARTESIAN_POINT('Ctrl Pts',(-113.888815670701,100.22768844038,-66.6754382808512));
#13124=CARTESIAN_POINT('Ctrl Pts',(-113.435498258322,100.22768844038,-66.413715350786));
#13125=CARTESIAN_POINT('Ctrl Pts',(-113.045853744828,100.22768844038,-66.1887539860318));
#13126=CARTESIAN_POINT('Ctrl Pts',(-112.64222922698,100.270378061999,-65.9097091373666));
#13127=CARTESIAN_POINT('Ctrl Pts',(-111.934430306435,100.476843984392,-65.2895980494646));
#13128=CARTESIAN_POINT('Ctrl Pts',(-111.630654997402,100.641526829723,-64.9483785209879));
#13129=CARTESIAN_POINT('Ctrl Pts',(-111.2369795781,101.04252635731,-64.3493295404366));
#13130=CARTESIAN_POINT('Ctrl Pts',(-111.099937593526,101.284167988039,-64.0558123049316));
#13131=CARTESIAN_POINT('Ctrl Pts',(-110.986598478824,101.851747702853,-63.5337079966479));
#13132=CARTESIAN_POINT('Ctrl Pts',(-111.009713416376,102.178321465582,-63.3059402798856));
#13133=CARTESIAN_POINT('Ctrl Pts',(-111.191412176548,102.807744434161,-62.9912287955964));
#13134=CARTESIAN_POINT('Ctrl Pts',(-111.351088823113,103.136138059265,-62.8857591987216));
#13135=CARTESIAN_POINT('Ctrl Pts',(-111.565481622863,103.438089404292,-62.8444992851724));
#13136=CARTESIAN_POINT('Ctrl Pts',(-111.565481622863,103.438089404292,-62.8444992851724));
#13137=CARTESIAN_POINT('Ctrl Pts',(-111.575188933326,103.451761204159,-62.8426311124026));
#13138=CARTESIAN_POINT('Ctrl Pts',(-111.585003582125,103.465381199048,-62.8408869585381));
#13139=CARTESIAN_POINT('Ctrl Pts',(-111.823912628857,103.792091077249,-62.8018507603263));
#13140=CARTESIAN_POINT('Ctrl Pts',(-112.112006606371,104.073708899229,-62.8337382694769));
#13141=CARTESIAN_POINT('Ctrl Pts',(-112.759808395975,104.553028941455,-62.9926274651217));
#13142=CARTESIAN_POINT('Ctrl Pts',(-113.170797750173,104.759746443146,-63.1481468200871));
#13143=CARTESIAN_POINT('Ctrl Pts',(-114.013782161377,105.021576797287,-63.5341097697223));
#13144=CARTESIAN_POINT('Ctrl Pts',(-114.445853744829,105.077430701572,-63.7638828554352));
#13145=CARTESIAN_POINT('Ctrl Pts',(-115.288815670702,105.077430701572,-64.2505671502546));
#13146=CARTESIAN_POINT('Ctrl Pts',(-115.767594076423,105.002693000391,-64.5533994185862));
#13147=CARTESIAN_POINT('Ctrl Pts',(-116.652114853179,104.700016463066,-65.1817663880356));
#13148=CARTESIAN_POINT('Ctrl Pts',(-117.058123820432,104.473289105623,-65.5075087398144));
#13149=CARTESIAN_POINT('Ctrl Pts',(-117.59419825037,103.990784840806,-66.0388312545589));
#13150=CARTESIAN_POINT('Ctrl Pts',(-117.798111636135,103.73410733426,-66.281258295277));
#13151=CARTESIAN_POINT('Ctrl Pts',(-117.971447315925,103.296228661322,-66.6204521442011));
#13152=CARTESIAN_POINT('Ctrl Pts',(-118.007599536035,103.14149423203,-66.7297304001928));
#13153=CARTESIAN_POINT('Ctrl Pts',(-118.025761966741,102.824004944285,-66.9316462349407));
#13154=CARTESIAN_POINT('Ctrl Pts',(-118.007691799887,102.661241838733,-67.0242780679549));
#13155=CARTESIAN_POINT('Ctrl Pts',(-117.914598780889,102.338758161266,-67.1855199066884));
#13156=CARTESIAN_POINT('Ctrl Pts',(-117.839876304636,102.180078121956,-67.2536096461054));
#13157=CARTESIAN_POINT('Ctrl Pts',(-117.643713131067,101.879175318306,-67.3610917996573));
#13158=CARTESIAN_POINT('Ctrl Pts',(-117.522786130607,101.736775618063,-67.4007763629426));
#13159=CARTESIAN_POINT('Ctrl Pts',(-117.386134507204,101.60505912631,-67.4270749801282));
#13160=CARTESIAN_POINT('',(-106.165171981646,103.438089404295,-86.8623521842208));
#13161=CARTESIAN_POINT('',(-100.344519097302,101.605059126314,-82.2797764892636));
#13162=CARTESIAN_POINT('Ctrl Pts',(-106.165171981646,103.438089404295,-86.862352184219));
#13163=CARTESIAN_POINT('Ctrl Pts',(-106.14419730415,103.462308875692,-86.8634802540479));
#13164=CARTESIAN_POINT('Ctrl Pts',(-106.12282827633,103.486302635371,-86.8641514184887));
#13165=CARTESIAN_POINT('Ctrl Pts',(-105.818714172361,103.818683816975,-86.8673779259697));
#13166=CARTESIAN_POINT('Ctrl Pts',(-105.472391325601,104.085740432872,-86.7940722130298));
#13167=CARTESIAN_POINT('Ctrl Pts',(-104.731279077633,104.539153956812,-86.5696833263198));
#13168=CARTESIAN_POINT('Ctrl Pts',(-104.271314809741,104.741671619492,-86.3849512882693));
#13169=CARTESIAN_POINT('Ctrl Pts',(-103.33961664048,105.01118751589,-85.9511255373707));
#13170=CARTESIAN_POINT('Ctrl Pts',(-102.867626486497,105.077430701576,-85.7021134546504));
#13171=CARTESIAN_POINT('Ctrl Pts',(-102.441408937237,105.077430701576,-85.4560366378519));
#13172=CARTESIAN_POINT('Ctrl Pts',(-102.014157839508,105.077430701576,-85.2093631015665));
#13173=CARTESIAN_POINT('Ctrl Pts',(-101.56105927878,105.010210941309,-84.9242504184528));
#13174=CARTESIAN_POINT('Ctrl Pts',(-100.752419784988,104.696117862631,-84.3353138424256));
#13175=CARTESIAN_POINT('Ctrl Pts',(-100.397371710978,104.448780822016,-84.0310608152941));
#13176=CARTESIAN_POINT('Ctrl Pts',(-99.9882037851011,103.92339933994,-83.5499074785033));
#13177=CARTESIAN_POINT('Ctrl Pts',(-99.8584603905707,103.660815277971,-83.3448119619325));
#13178=CARTESIAN_POINT('Ctrl Pts',(-99.7452298798465,103.091082457567,-82.9637606339507));
#13179=CARTESIAN_POINT('Ctrl Pts',(-99.7621917782077,102.784236407494,-82.7872192164191));
#13180=CARTESIAN_POINT('Ctrl Pts',(-99.9262957445862,102.215763592511,-82.502982808928));
#13181=CARTESIAN_POINT('Ctrl Pts',(-100.082544658828,101.922589786887,-82.379514298611));
#13182=CARTESIAN_POINT('Ctrl Pts',(-100.312341841756,101.642706629092,-82.2911817419664));
#13183=CARTESIAN_POINT('Ctrl Pts',(-100.328291840436,101.623796748554,-82.2853723510623));
#13184=CARTESIAN_POINT('Ctrl Pts',(-100.344519097301,101.605059126315,-82.2797764892642));
#13185=CARTESIAN_POINT('Ctrl Pts',(-100.344519097301,101.605059126315,-82.2797764892642));
#13186=CARTESIAN_POINT('Ctrl Pts',(-100.550215520806,101.367541355351,-82.2088434432281));
#13187=CARTESIAN_POINT('Ctrl Pts',(-100.802602048525,101.15899254472,-82.1740857015096));
#13188=CARTESIAN_POINT('Ctrl Pts',(-101.47214666584,100.72565116497,-82.1694959867722));
#13189=CARTESIAN_POINT('Ctrl Pts',(-101.955786523501,100.527533200142,-82.2510215111824));
#13190=CARTESIAN_POINT('Ctrl Pts',(-102.926860882229,100.278935400847,-82.5586126482226));
#13191=CARTESIAN_POINT('Ctrl Pts',(-103.414157839508,100.227688440382,-82.784491970971));
#13192=CARTESIAN_POINT('Ctrl Pts',(-104.267626486497,100.227688440382,-83.2772423240549));
#13193=CARTESIAN_POINT('Ctrl Pts',(-104.705846427788,100.278428703028,-83.5847461309404));
#13194=CARTESIAN_POINT('Ctrl Pts',(-105.498304549662,100.491254479672,-84.2597427183605));
#13195=CARTESIAN_POINT('Ctrl Pts',(-105.853076223232,100.653134652889,-84.6266736743588));
#13196=CARTESIAN_POINT('Ctrl Pts',(-106.353797244182,101.032460766724,-85.2674323799564));
#13197=CARTESIAN_POINT('Ctrl Pts',(-106.557061980701,101.260971981571,-85.5885220082683));
#13198=CARTESIAN_POINT('Ctrl Pts',(-106.72625467127,101.679226130855,-86.024626674228));
#13199=CARTESIAN_POINT('Ctrl Pts',(-106.760576424903,101.831187432809,-86.1626137356242));
#13200=CARTESIAN_POINT('Ctrl Pts',(-106.774196861679,102.153837950614,-86.4089088160002));
#13201=CARTESIAN_POINT('Ctrl Pts',(-106.753460724005,102.324558208363,-86.5171780914983));
#13202=CARTESIAN_POINT('Ctrl Pts',(-106.652169358375,102.675441791642,-86.692619883138));
#13203=CARTESIAN_POINT('Ctrl Pts',(-106.572948453007,102.850982888141,-86.7574812847633));
#13204=CARTESIAN_POINT('Ctrl Pts',(-106.38376792248,103.164953280743,-86.8360360636708));
#13205=CARTESIAN_POINT('Ctrl Pts',(-106.28046465974,103.304960886828,-86.8561514599566));
#13206=CARTESIAN_POINT('Ctrl Pts',(-106.165171981646,103.438089404295,-86.862352184219));
#13207=CARTESIAN_POINT('',(-105.707515158216,101.445788778226,-60.813667453584));
#13208=CARTESIAN_POINT('',(-101.324821922316,103.6146594521,-56.8374045514775));
#13209=CARTESIAN_POINT('Ctrl Pts',(-105.707515158216,101.445788778225,-60.8136674535836));
#13210=CARTESIAN_POINT('Ctrl Pts',(-105.483577684551,101.227887906321,-60.8640309956986));
#13211=CARTESIAN_POINT('Ctrl Pts',(-105.222582053125,101.039304544329,-60.8807352012508));
#13212=CARTESIAN_POINT('Ctrl Pts',(-104.602960841079,100.67854055414,-60.8556299182567));
#13213=CARTESIAN_POINT('Ctrl Pts',(-104.1892589951,100.508020898325,-60.7865580098289));
#13214=CARTESIAN_POINT('Ctrl Pts',(-103.362197532696,100.282687776782,-60.5388045693685));
#13215=CARTESIAN_POINT('Ctrl Pts',(-102.949106981883,100.22768844038,-60.359394524506));
#13216=CARTESIAN_POINT('Ctrl Pts',(-102.587887471937,100.22768844038,-60.1508443432025));
#13217=CARTESIAN_POINT('Ctrl Pts',(-102.254878013721,100.22768844038,-59.9585812428588));
#13218=CARTESIAN_POINT('Ctrl Pts',(-101.918162195562,100.275039954704,-59.7132182406853));
#13219=CARTESIAN_POINT('Ctrl Pts',(-101.348088424631,100.488116881772,-59.166211609912));
#13220=CARTESIAN_POINT('Ctrl Pts',(-101.114826914581,100.65473625473,-58.8648160959221));
#13221=CARTESIAN_POINT('Ctrl Pts',(-100.809047976543,101.052694817512,-58.3193334032543));
#13222=CARTESIAN_POINT('Ctrl Pts',(-100.708587237918,101.302215526292,-58.04101395854));
#13223=CARTESIAN_POINT('Ctrl Pts',(-100.646124764096,101.871223563749,-57.5488477901271));
#13224=CARTESIAN_POINT('Ctrl Pts',(-100.683391349424,102.19108472861,-57.3355266127738));
#13225=CARTESIAN_POINT('Ctrl Pts',(-100.861743664517,102.808915271389,-57.0266113413844));
#13226=CARTESIAN_POINT('Ctrl Pts',(-101.013824739271,103.144973641637,-56.9119727511829));
#13227=CARTESIAN_POINT('Ctrl Pts',(-101.251985600091,103.511086021696,-56.8502538040771));
#13228=CARTESIAN_POINT('Ctrl Pts',(-101.287761408094,103.563290529642,-56.8430050519095));
#13229=CARTESIAN_POINT('Ctrl Pts',(-101.324821922315,103.614659452099,-56.8374045514776));
#13230=CARTESIAN_POINT('Ctrl Pts',(-101.324821922315,103.614659452099,-56.8374045514776));
#13231=CARTESIAN_POINT('Ctrl Pts',(-101.507571534895,103.867965453781,-56.8097878465912));
#13232=CARTESIAN_POINT('Ctrl Pts',(-101.722903603191,104.100150075329,-56.8237200261498));
#13233=CARTESIAN_POINT('Ctrl Pts',(-102.23560907329,104.537239540928,-56.9235644528227));
#13234=CARTESIAN_POINT('Ctrl Pts',(-102.577115242381,104.745590666186,-57.0374747177044));
#13235=CARTESIAN_POINT('Ctrl Pts',(-103.286625217418,105.015534918971,-57.3429707585513));
#13236=CARTESIAN_POINT('Ctrl Pts',(-103.654878013722,105.077430701572,-57.5337101122621));
#13237=CARTESIAN_POINT('Ctrl Pts',(-104.349106981883,105.077430701572,-57.9345233939092));
#13238=CARTESIAN_POINT('Ctrl Pts',(-104.725589216724,105.005615111484,-58.1773409020166));
#13239=CARTESIAN_POINT('Ctrl Pts',(-105.40533608587,104.720635512592,-58.6802507026948));
#13240=CARTESIAN_POINT('Ctrl Pts',(-105.708442531058,104.5080414619,-58.9408794643765));
#13241=CARTESIAN_POINT('Ctrl Pts',(-106.134628803274,104.039966782051,-59.3986735814598));
#13242=CARTESIAN_POINT('Ctrl Pts',(-106.301658407902,103.762601478164,-59.628755601445));
#13243=CARTESIAN_POINT('Ctrl Pts',(-106.466981515918,103.150363245665,-60.0574871392715));
#13244=CARTESIAN_POINT('Ctrl Pts',(-106.463597321879,102.815336528851,-60.256562220115));
#13245=CARTESIAN_POINT('Ctrl Pts',(-106.281537692062,102.184663471148,-60.5718987489666));
#13246=CARTESIAN_POINT('Ctrl Pts',(-106.096327018674,101.866378403104,-60.6994795605523));
#13247=CARTESIAN_POINT('Ctrl Pts',(-105.801011946827,101.53963142162,-60.790807331965));
#13248=CARTESIAN_POINT('Ctrl Pts',(-105.755075673419,101.492067221763,-60.8029710928037));
#13249=CARTESIAN_POINT('Ctrl Pts',(-105.707515158216,101.445788778225,-60.8136674535836));
#13250=CARTESIAN_POINT('',(-94.501534612098,103.614659452104,-80.2229951080884));
#13251=CARTESIAN_POINT('',(-90.1188413761952,101.445788778232,-76.2467322059816));
#13252=CARTESIAN_POINT('Ctrl Pts',(-94.5015346120983,103.614659452105,-80.222995108087));
#13253=CARTESIAN_POINT('Ctrl Pts',(-94.2999319259417,103.85835031517,-80.2346736634614));
#13254=CARTESIAN_POINT('Ctrl Pts',(-94.0660003649607,104.078184573876,-80.204501523942));
#13255=CARTESIAN_POINT('Ctrl Pts',(-93.506215357663,104.508041461903,-80.0757568941915));
#13256=CARTESIAN_POINT('Ctrl Pts',(-93.1289510064958,104.720635512595,-79.9435733934488));
#13257=CARTESIAN_POINT('Ctrl Pts',(-92.353544908723,105.005615111488,-79.6063502369639));
#13258=CARTESIAN_POINT('Ctrl Pts',(-91.9550176607982,105.077430701576,-79.4017158115723));
#13259=CARTESIAN_POINT('Ctrl Pts',(-91.5937981508529,105.077430701576,-79.1931656302689));
#13260=CARTESIAN_POINT('Ctrl Pts',(-91.2445310553966,105.077430701576,-78.9915161786881));
#13261=CARTESIAN_POINT('Ctrl Pts',(-90.8794457263923,105.009294935457,-78.75672916701));
#13262=CARTESIAN_POINT('Ctrl Pts',(-90.2394279750154,104.71379978534,-78.2726325195484));
#13263=CARTESIAN_POINT('Ctrl Pts',(-89.9651725619102,104.486205632632,-78.0225716794456));
#13264=CARTESIAN_POINT('Ctrl Pts',(-89.615152325688,103.992202355958,-77.5948073108704));
#13265=CARTESIAN_POINT('Ctrl Pts',(-89.4966157452444,103.711875068197,-77.3893068873646));
#13266=CARTESIAN_POINT('Ctrl Pts',(-89.4038756583846,103.11192693574,-77.0059525649689));
#13267=CARTESIAN_POINT('Ctrl Pts',(-89.4297352858526,102.792723417415,-76.8274306857825));
#13268=CARTESIAN_POINT('Ctrl Pts',(-89.5987392296941,102.207276582589,-76.5347072683697));
#13269=CARTESIAN_POINT('Ctrl Pts',(-89.7529823542094,101.902585866878,-76.4012820305381));
#13270=CARTESIAN_POINT('Ctrl Pts',(-90.0135013341837,101.566233275656,-76.2843454877329));
#13271=CARTESIAN_POINT('Ctrl Pts',(-90.0649390949408,101.505064596095,-76.2644831614807));
#13272=CARTESIAN_POINT('Ctrl Pts',(-90.1188413761922,101.445788778236,-76.2467322059833));
#13273=CARTESIAN_POINT('Ctrl Pts',(-90.1188413761922,101.445788778236,-76.2467322059833));
#13274=CARTESIAN_POINT('Ctrl Pts',(-90.3002565105157,101.246288307949,-76.1869890578052));
#13275=CARTESIAN_POINT('Ctrl Pts',(-90.5105127919593,101.068816696773,-76.1519939958911));
#13276=CARTESIAN_POINT('Ctrl Pts',(-91.0593017712658,100.696030871333,-76.1274842987972));
#13277=CARTESIAN_POINT('Ctrl Pts',(-91.4519661767371,100.513444242339,-76.1724547480489));
#13278=CARTESIAN_POINT('Ctrl Pts',(-92.2447448611874,100.279759997467,-76.3919616980159));
#13279=CARTESIAN_POINT('Ctrl Pts',(-92.6445310553966,100.227688440383,-76.5666450480926));
#13280=CARTESIAN_POINT('Ctrl Pts',(-93.3550176607982,100.227688440383,-76.9768446809768));
#13281=CARTESIAN_POINT('Ctrl Pts',(-93.7169365927499,100.282687776784,-77.2448865696132));
#13282=CARTESIAN_POINT('Ctrl Pts',(-94.3450280972656,100.508020898327,-77.8372660863158));
#13283=CARTESIAN_POINT('Ctrl Pts',(-94.6116970476415,100.678540554143,-78.1610064403122));
#13284=CARTESIAN_POINT('Ctrl Pts',(-94.9727271872904,101.071379412638,-78.7316542894256));
#13285=CARTESIAN_POINT('Ctrl Pts',(-95.1064606462321,101.310297639174,-79.0194069254365));
#13286=CARTESIAN_POINT('Ctrl Pts',(-95.2231499598568,101.866378403107,-79.5323746661135));
#13287=CARTESIAN_POINT('Ctrl Pts',(-95.2052670726821,102.184663471151,-79.7565622201121));
#13288=CARTESIAN_POINT('Ctrl Pts',(-95.0232074428643,102.815336528854,-80.0718987489636));
#13289=CARTESIAN_POINT('Ctrl Pts',(-94.8524954626127,103.150363245668,-80.174367087394));
#13290=CARTESIAN_POINT('Ctrl Pts',(-94.5857570770073,103.510107742139,-80.2161985863255));
#13291=CARTESIAN_POINT('Ctrl Pts',(-94.5443515978532,103.562903652559,-80.2205147813183));
#13292=CARTESIAN_POINT('Ctrl Pts',(-94.5015346120983,103.614659452105,-80.222995108087));
#13293=CARTESIAN_POINT('',(-94.2209929096256,101.354811290699,-54.2576156201439));
#13294=CARTESIAN_POINT('',(-90.5178421019398,103.716919354992,-50.5448617949466));
#13295=CARTESIAN_POINT('Ctrl Pts',(-94.2209929096261,101.354811290699,-54.2576156201434));
#13296=CARTESIAN_POINT('Ctrl Pts',(-94.0304505856294,101.165865871972,-54.3062458592498));
#13297=CARTESIAN_POINT('Ctrl Pts',(-93.8147279386984,100.999081132478,-54.3308652529223));
#13298=CARTESIAN_POINT('Ctrl Pts',(-93.2853347608051,100.664686636251,-54.335231850713));
#13299=CARTESIAN_POINT('Ctrl Pts',(-92.9240531847944,100.499668449628,-54.2909952556545));
#13300=CARTESIAN_POINT('Ctrl Pts',(-92.1976667058189,100.281331189612,-54.0944571890166));
#13301=CARTESIAN_POINT('Ctrl Pts',(-91.8328571384615,100.22768844038,-53.9414246850278));
#13302=CARTESIAN_POINT('Ctrl Pts',(-91.5141993333915,100.22768844038,-53.7574475154913));
#13303=CARTESIAN_POINT('Ctrl Pts',(-91.1998056536407,100.22768844038,-53.5759322398556));
#13304=CARTESIAN_POINT('Ctrl Pts',(-90.8886903708508,100.280334555034,-53.3396967948896));
#13305=CARTESIAN_POINT('Ctrl Pts',(-90.3733823362884,100.504055421459,-52.8139276391242));
#13306=CARTESIAN_POINT('Ctrl Pts',(-90.1688519647511,100.67573731595,-52.5249835715961));
#13307=CARTESIAN_POINT('Ctrl Pts',(-89.9037680431757,101.07557755986,-52.0026890248464));
#13308=CARTESIAN_POINT('Ctrl Pts',(-89.8203132445372,101.325643828305,-51.7350194741849));
#13309=CARTESIAN_POINT('Ctrl Pts',(-89.7787639540569,101.887795138889,-51.2622217134503));
#13310=CARTESIAN_POINT('Ctrl Pts',(-89.8201747804601,102.200227598979,-51.0575503555047));
#13311=CARTESIAN_POINT('Ctrl Pts',(-89.9932484568848,102.799772401019,-50.7577779544845));
#13312=CARTESIAN_POINT('Ctrl Pts',(-90.1366138563365,103.127423563352,-50.6424075012184));
#13313=CARTESIAN_POINT('Ctrl Pts',(-90.3868899039983,103.531966317969,-50.5657018885759));
#13314=CARTESIAN_POINT('Ctrl Pts',(-90.4505284239739,103.625948972014,-50.5527189917843));
#13315=CARTESIAN_POINT('Ctrl Pts',(-90.5178421019398,103.716919354992,-50.5448617949466));
#13316=CARTESIAN_POINT('Ctrl Pts',(-90.5178421019398,103.716919354992,-50.5448617949466));
#13317=CARTESIAN_POINT('Ctrl Pts',(-90.6677586076694,103.919522486378,-50.5273627734945));
#13318=CARTESIAN_POINT('Ctrl Pts',(-90.8363800498654,104.106877932436,-50.5357972502939));
#13319=CARTESIAN_POINT('Ctrl Pts',(-91.2761732604758,104.511610804944,-50.6070468270981));
#13320=CARTESIAN_POINT('Ctrl Pts',(-91.5920360022583,104.725595554037,-50.7031575728346));
#13321=CARTESIAN_POINT('Ctrl Pts',(-92.2536368706955,105.008647929721,-50.9755401075456));
#13322=CARTESIAN_POINT('Ctrl Pts',(-92.5998056536411,105.077430701572,-51.1510611092587));
#13323=CARTESIAN_POINT('Ctrl Pts',(-93.232857138462,105.077430701572,-51.5165535544309));
#13324=CARTESIAN_POINT('Ctrl Pts',(-93.5619700271323,105.00741652851,-51.7314145195672));
#13325=CARTESIAN_POINT('Ctrl Pts',(-94.1455671289826,104.731116876602,-52.1752710421669));
#13326=CARTESIAN_POINT('Ctrl Pts',(-94.3998110409153,104.525345718212,-52.4049023097321));
#13327=CARTESIAN_POINT('Ctrl Pts',(-94.768377540354,104.0613168212,-52.8259509372149));
#13328=CARTESIAN_POINT('Ctrl Pts',(-94.9105232806575,103.7725092302,-53.0468145506106));
#13329=CARTESIAN_POINT('Ctrl Pts',(-95.0354212815802,103.14720818058,-53.4590643079669));
#13330=CARTESIAN_POINT('Ctrl Pts',(-95.0172814114049,102.810893242388,-53.6509908389482));
#13331=CARTESIAN_POINT('Ctrl Pts',(-94.8377871142222,102.18910675761,-53.9618840813374));
#13332=CARTESIAN_POINT('Ctrl Pts',(-94.66647754768,101.869149596082,-54.0980936002161));
#13333=CARTESIAN_POINT('Ctrl Pts',(-94.365959399355,101.505588017214,-54.2160961273275));
#13334=CARTESIAN_POINT('Ctrl Pts',(-94.2953494579818,101.428544668509,-54.238638331267));
#13335=CARTESIAN_POINT('Ctrl Pts',(-94.2209929096261,101.354811290699,-54.2576156201434));
#13336=CARTESIAN_POINT('',(-83.0247832218288,103.716919354995,-73.6500196516034));
#13337=CARTESIAN_POINT('',(-79.3216324141422,101.354811290702,-69.9372658264059));
#13338=CARTESIAN_POINT('Ctrl Pts',(-83.0247832218292,103.716919354995,-73.6500196516021));
#13339=CARTESIAN_POINT('Ctrl Pts',(-82.8561874835582,103.929460895585,-73.6618384029087));
#13340=CARTESIAN_POINT('Ctrl Pts',(-82.6660644120803,104.123947093647,-73.6439402061671));
#13341=CARTESIAN_POINT('Ctrl Pts',(-82.1939330584629,104.523769595123,-73.5508930043753));
#13342=CARTESIAN_POINT('Ctrl Pts',(-81.8675496354975,104.73010984644,-73.445550762439));
#13343=CARTESIAN_POINT('Ctrl Pts',(-81.1904340361545,105.007198663853,-73.1618575252943));
#13344=CARTESIAN_POINT('Ctrl Pts',(-80.8392691645201,105.077430701576,-72.9840354250022));
#13345=CARTESIAN_POINT('Ctrl Pts',(-80.5201100123077,105.077430701576,-72.799768802558));
#13346=CARTESIAN_POINT('Ctrl Pts',(-80.2107074631239,105.077430701576,-72.6211351574988));
#13347=CARTESIAN_POINT('Ctrl Pts',(-79.8902928105569,105.010817414927,-72.4125520697033));
#13348=CARTESIAN_POINT('Ctrl Pts',(-79.3296459208272,104.735983399352,-71.9826313276384));
#13349=CARTESIAN_POINT('Ctrl Pts',(-79.0898300656876,104.528017888669,-71.760587957699));
#13350=CARTESIAN_POINT('Ctrl Pts',(-78.7510680657571,104.056494164301,-71.353383279585));
#13351=CARTESIAN_POINT('Ctrl Pts',(-78.6282785579301,103.763711210128,-71.1414137376349));
#13352=CARTESIAN_POINT('Ctrl Pts',(-78.5328756547392,103.137634877854,-70.745080894813));
#13353=CARTESIAN_POINT('Ctrl Pts',(-78.5604078289852,102.804749283705,-70.5600387968433));
#13354=CARTESIAN_POINT('Ctrl Pts',(-78.7363549099663,102.1952507163,-70.2552895131407));
#13355=CARTESIAN_POINT('Ctrl Pts',(-78.8964707374473,101.878104564589,-70.1153157381806));
#13356=CARTESIAN_POINT('Ctrl Pts',(-79.1804605765672,101.511189981574,-69.9855724361914));
#13357=CARTESIAN_POINT('Ctrl Pts',(-79.2490780626133,101.431324815456,-69.9596178450133));
#13358=CARTESIAN_POINT('Ctrl Pts',(-79.3216324141422,101.354811290702,-69.9372658264059));
#13359=CARTESIAN_POINT('Ctrl Pts',(-79.3216324141422,101.354811290702,-69.9372658264059));
#13360=CARTESIAN_POINT('Ctrl Pts',(-79.4994951487113,101.167242875335,-69.8824711646265));
#13361=CARTESIAN_POINT('Ctrl Pts',(-79.7016131069151,101.000214480644,-69.8498916678611));
#13362=CARTESIAN_POINT('Ctrl Pts',(-80.2057230797504,100.662451096332,-69.8278045615312));
#13363=CARTESIAN_POINT('Ctrl Pts',(-80.5536874604562,100.495779124926,-69.8625291904263));
#13364=CARTESIAN_POINT('Ctrl Pts',(-81.2563406796862,100.27868878512,-70.0464877548005));
#13365=CARTESIAN_POINT('Ctrl Pts',(-81.6107074631236,100.227688440383,-70.1962640269031));
#13366=CARTESIAN_POINT('Ctrl Pts',(-82.2392691645199,100.227688440383,-70.5591642944065));
#13367=CARTESIAN_POINT('Ctrl Pts',(-82.5546266768382,100.281496733901,-70.7990065603189));
#13368=CARTESIAN_POINT('Ctrl Pts',(-83.0885412363331,100.500470869914,-71.330731274177));
#13369=CARTESIAN_POINT('Ctrl Pts',(-83.3075860460983,100.665962481951,-71.6219894477902));
#13370=CARTESIAN_POINT('Ctrl Pts',(-83.6098374691532,101.054698410516,-72.1567503717173));
#13371=CARTESIAN_POINT('Ctrl Pts',(-83.7166215744316,101.303006298545,-72.4375565865388));
#13372=CARTESIAN_POINT('Ctrl Pts',(-83.7911705443989,101.870113330836,-72.9351916366745));
#13373=CARTESIAN_POINT('Ctrl Pts',(-83.7588055350932,102.189611224737,-73.1512430725076));
#13374=CARTESIAN_POINT('Ctrl Pts',(-83.5796024921405,102.810388775268,-73.4616318477727));
#13375=CARTESIAN_POINT('Ctrl Pts',(-83.4227987210069,103.14619075922,-73.5732303508662));
#13376=CARTESIAN_POINT('Ctrl Pts',(-83.1543827768569,103.546695163547,-73.6361875753525));
#13377=CARTESIAN_POINT('Ctrl Pts',(-83.0912106178557,103.633177136873,-73.6453630162586));
#13378=CARTESIAN_POINT('Ctrl Pts',(-83.0247832218292,103.716919354995,-73.6500196516021));
#13379=CARTESIAN_POINT('',(-79.2724338250639,100.514077983564,-46.3961169753473));
#13380=CARTESIAN_POINT('',(-82.9097405209592,104.714077983563,-45.6961169753459));
#13381=CARTESIAN_POINT('Ctrl Pts',(-79.2724338250643,100.514077983563,-46.3961169753468));
#13382=CARTESIAN_POINT('Ctrl Pts',(-79.1265511423845,100.610404906306,-46.2160498567682));
#13383=CARTESIAN_POINT('Ctrl Pts',(-79.0063377502804,100.729412390803,-46.0312428512855));
#13384=CARTESIAN_POINT('Ctrl Pts',(-78.7783882480642,101.056823805357,-45.5960981587349));
#13385=CARTESIAN_POINT('Ctrl Pts',(-78.6879980806413,101.308592332844,-45.3220312346838));
#13386=CARTESIAN_POINT('Ctrl Pts',(-78.637346637553,101.87720020589,-44.8375673373119));
#13387=CARTESIAN_POINT('Ctrl Pts',(-78.6768221832288,102.194506798829,-44.627746600585));
#13388=CARTESIAN_POINT('Ctrl Pts',(-78.8531987651598,102.805493201169,-44.3222533994151));
#13389=CARTESIAN_POINT('Ctrl Pts',(-79.001482969892,103.138605462875,-44.2068647088189));
#13390=CARTESIAN_POINT('Ctrl Pts',(-79.3969069246043,103.764324604201,-44.094165099005));
#13391=CARTESIAN_POINT('Ctrl Pts',(-79.6443545210792,104.056618970362,-44.0962005762319));
#13392=CARTESIAN_POINT('Ctrl Pts',(-80.1647562293486,104.52433820779,-44.1867417540882));
#13393=CARTESIAN_POINT('Ctrl Pts',(-80.4728761101798,104.731264722065,-44.2812762970742));
#13394=CARTESIAN_POINT('Ctrl Pts',(-81.1163900166925,105.008060588784,-44.5457120366282));
#13395=CARTESIAN_POINT('Ctrl Pts',(-81.4522447708355,105.077430701572,-44.7150138327633));
#13396=CARTESIAN_POINT('Ctrl Pts',(-82.0632775106341,105.077430701572,-45.0677937495697));
#13397=CARTESIAN_POINT('Ctrl Pts',(-82.3778245440648,105.008060588784,-45.2740016005717));
#13398=CARTESIAN_POINT('Ctrl Pts',(-82.7431217757092,104.824474558593,-45.5559387185791));
#13399=CARTESIAN_POINT('Ctrl Pts',(-82.8290587463787,104.772275635182,-45.6260680866036));
#13400=CARTESIAN_POINT('Ctrl Pts',(-82.9097405209591,104.714077983563,-45.6961169753458));
#13401=CARTESIAN_POINT('Ctrl Pts',(-82.9097405209591,104.714077983563,-45.6961169753458));
#13402=CARTESIAN_POINT('Ctrl Pts',(-83.0761634408585,104.594033237844,-45.8406073594606));
#13403=CARTESIAN_POINT('Ctrl Pts',(-83.2198007296756,104.447978167203,-45.9848429857255));
#13404=CARTESIAN_POINT('Ctrl Pts',(-83.5031306358671,104.056618970362,-46.3240660048471));
#13405=CARTESIAN_POINT('Ctrl Pts',(-83.6286172090919,103.764324604201,-46.5373441708864));
#13406=CARTESIAN_POINT('Ctrl Pts',(-83.7287284613526,103.138605462875,-46.936141165839));
#13407=CARTESIAN_POINT('Ctrl Pts',(-83.7029410263529,102.805493201169,-47.1222533994152));
#13408=CARTESIAN_POINT('Ctrl Pts',(-83.5265644444219,102.194506798829,-47.427746600585));
#13409=CARTESIAN_POINT('Ctrl Pts',(-83.3645921290135,101.87720020589,-47.5668437943321));
#13410=CARTESIAN_POINT('Ctrl Pts',(-82.9197083651289,101.308592332844,-47.7652103065652));
#13411=CARTESIAN_POINT('Ctrl Pts',(-82.6371643628521,101.056823805357,-47.8239635873502));
#13412=CARTESIAN_POINT('Ctrl Pts',(-82.0505767043741,100.665529520269,-47.8480598380025));
#13413=CARTESIAN_POINT('Ctrl Pts',(-81.7069979829943,100.499547348265,-47.8149418084238));
#13414=CARTESIAN_POINT('Ctrl Pts',(-81.0131896142114,100.280826524207,-47.637618632861));
#13415=CARTESIAN_POINT('Ctrl Pts',(-80.6632775106336,100.227688440379,-47.4926648801669));
#13416=CARTESIAN_POINT('Ctrl Pts',(-80.3577611407344,100.227688440379,-47.3162749217637));
#13417=CARTESIAN_POINT('Ctrl Pts',(-80.0522447708351,100.227688440379,-47.1398849633606));
#13418=CARTESIAN_POINT('Ctrl Pts',(-79.7517550868392,100.280826524207,-46.9093290689175));
#13419=CARTESIAN_POINT('Ctrl Pts',(-79.4198158701761,100.42589403654,-46.5696141741228));
#13420=CARTESIAN_POINT('Ctrl Pts',(-79.3431576996741,100.467378724402,-46.4834134527748));
#13421=CARTESIAN_POINT('Ctrl Pts',(-79.2724338250643,100.514077983563,-46.3961169753468));
#13422=CARTESIAN_POINT('',(-68.2116924394259,104.714077983566,-65.5538830246524));
#13423=CARTESIAN_POINT('',(-71.8489991353209,100.514077983566,-64.8538830246516));
#13424=CARTESIAN_POINT('Ctrl Pts',(-68.2116924394265,104.714077983567,-65.5538830246511));
#13425=CARTESIAN_POINT('Ctrl Pts',(-68.0452695195272,104.594033237848,-65.4093926405365));
#13426=CARTESIAN_POINT('Ctrl Pts',(-67.9016322307103,104.447978167207,-65.2651570142717));
#13427=CARTESIAN_POINT('Ctrl Pts',(-67.6183023245187,104.056618970366,-64.9259339951503));
#13428=CARTESIAN_POINT('Ctrl Pts',(-67.4928157512939,103.764324604205,-64.7126558291111));
#13429=CARTESIAN_POINT('Ctrl Pts',(-67.3927044990331,103.138605462879,-64.3138588341587));
#13430=CARTESIAN_POINT('Ctrl Pts',(-67.4184919340327,102.805493201172,-64.1277466005826));
#13431=CARTESIAN_POINT('Ctrl Pts',(-67.5948685159636,102.194506798833,-63.8222533994129));
#13432=CARTESIAN_POINT('Ctrl Pts',(-67.7568408313719,101.877200205893,-63.683156205666));
#13433=CARTESIAN_POINT('Ctrl Pts',(-68.2017245952565,101.308592332847,-63.484789693433));
#13434=CARTESIAN_POINT('Ctrl Pts',(-68.4842685975332,101.056823805361,-63.4260364126481));
#13435=CARTESIAN_POINT('Ctrl Pts',(-69.0708562560112,100.665529520272,-63.4019401619959));
#13436=CARTESIAN_POINT('Ctrl Pts',(-69.4144349773908,100.499547348269,-63.4350581915746));
#13437=CARTESIAN_POINT('Ctrl Pts',(-70.1082433461736,100.28082652421,-63.6123813671375));
#13438=CARTESIAN_POINT('Ctrl Pts',(-70.4581554497515,100.227688440383,-63.7573351198316));
#13439=CARTESIAN_POINT('Ctrl Pts',(-71.0691881895501,100.227688440383,-64.110115036638));
#13440=CARTESIAN_POINT('Ctrl Pts',(-71.369677873546,100.28082652421,-64.340670931081));
#13441=CARTESIAN_POINT('Ctrl Pts',(-71.701617090209,100.425894036543,-64.6803858258755));
#13442=CARTESIAN_POINT('Ctrl Pts',(-71.7782752607111,100.467378724405,-64.7665865472236));
#13443=CARTESIAN_POINT('Ctrl Pts',(-71.8489991353208,100.514077983566,-64.8538830246515));
#13444=CARTESIAN_POINT('Ctrl Pts',(-71.8489991353208,100.514077983566,-64.8538830246515));
#13445=CARTESIAN_POINT('Ctrl Pts',(-71.9948818180007,100.61040490631,-65.0339501432301));
#13446=CARTESIAN_POINT('Ctrl Pts',(-72.1150952101049,100.729412390806,-65.2187571487129));
#13447=CARTESIAN_POINT('Ctrl Pts',(-72.3430447123212,101.056823805361,-65.6539018412633));
#13448=CARTESIAN_POINT('Ctrl Pts',(-72.4334348797441,101.308592332847,-65.9279687653144));
#13449=CARTESIAN_POINT('Ctrl Pts',(-72.4840863228325,101.877200205893,-66.4124326626861));
#13450=CARTESIAN_POINT('Ctrl Pts',(-72.4446107771567,102.194506798833,-66.622253399413));
#13451=CARTESIAN_POINT('Ctrl Pts',(-72.2682341952258,102.805493201172,-66.9277466005826));
#13452=CARTESIAN_POINT('Ctrl Pts',(-72.1199499904937,103.138605462879,-67.0431352911788));
#13453=CARTESIAN_POINT('Ctrl Pts',(-71.7245260357815,103.764324604205,-67.1558349009925));
#13454=CARTESIAN_POINT('Ctrl Pts',(-71.4770784393067,104.056618970366,-67.1537994237656));
#13455=CARTESIAN_POINT('Ctrl Pts',(-70.9566767310373,104.524338207794,-67.0632582459091));
#13456=CARTESIAN_POINT('Ctrl Pts',(-70.6485568502061,104.731264722069,-66.968723702923));
#13457=CARTESIAN_POINT('Ctrl Pts',(-70.0050429436934,105.008060588788,-66.7042879633689));
#13458=CARTESIAN_POINT('Ctrl Pts',(-69.6691881895505,105.077430701576,-66.5349861672338));
#13459=CARTESIAN_POINT('Ctrl Pts',(-69.3636718196512,105.077430701576,-66.3585962088306));
#13460=CARTESIAN_POINT('Ctrl Pts',(-69.0581554497519,105.077430701576,-66.1822062504275));
#13461=CARTESIAN_POINT('Ctrl Pts',(-68.7436084163211,105.008060588788,-65.9759983994254));
#13462=CARTESIAN_POINT('Ctrl Pts',(-68.3783111846766,104.824474558597,-65.694061281418));
#13463=CARTESIAN_POINT('Ctrl Pts',(-68.292374214007,104.772275635186,-65.6239319133934));
#13464=CARTESIAN_POINT('Ctrl Pts',(-68.2116924394265,104.714077983567,-65.5538830246511));
#13465=CARTESIAN_POINT('',(-112.569378637745,121.956851469395,-75.7699408736866));
#13466=CARTESIAN_POINT('',(-105.161274966764,121.956851469395,-73.9369105957041));
#13467=CARTESIAN_POINT('Ctrl Pts',(-112.569378637745,121.956851469395,-75.7699408736867));
#13468=CARTESIAN_POINT('Ctrl Pts',(-112.569272008943,121.95672834506,-75.7681386924676));
#13469=CARTESIAN_POINT('Ctrl Pts',(-112.569163342679,121.956605035935,-75.7663364623398));
#13470=CARTESIAN_POINT('Ctrl Pts',(-112.545386428826,121.930081208774,-75.3792452325324));
#13471=CARTESIAN_POINT('Ctrl Pts',(-112.425619842949,121.895265649918,-74.9910716591131));
#13472=CARTESIAN_POINT('Ctrl Pts',(-112.050450493293,121.820378366244,-74.1810533701236));
#13473=CARTESIAN_POINT('Ctrl Pts',(-111.722843184654,121.775514411454,-73.719515362228));
#13474=CARTESIAN_POINT('Ctrl Pts',(-110.943904850608,121.712442638456,-72.9082742376171));
#13475=CARTESIAN_POINT('Ctrl Pts',(-110.491771010159,121.694880858045,-72.5592922284894));
#13476=CARTESIAN_POINT('Ctrl Pts',(-110.03845359778,121.694880858045,-72.2975692984242));
#13477=CARTESIAN_POINT('Ctrl Pts',(-109.648809084286,121.694880858045,-72.07260793367));
#13478=CARTESIAN_POINT('Ctrl Pts',(-109.196813666427,121.708045140711,-71.8773439414328));
#13479=CARTESIAN_POINT('Ctrl Pts',(-108.262263007713,121.76340957246,-71.6499783847423));
#13480=CARTESIAN_POINT('Ctrl Pts',(-107.779465090809,121.805444228819,-71.6188351088017));
#13481=CARTESIAN_POINT('Ctrl Pts',(-106.970686338396,121.883764743458,-71.7387661915901));
#13482=CARTESIAN_POINT('Ctrl Pts',(-106.589756165829,121.923740934709,-71.8676756890549));
#13483=CARTESIAN_POINT('Ctrl Pts',(-105.93403329749,121.982452032228,-72.2850075992705));
#13484=CARTESIAN_POINT('Ctrl Pts',(-105.659130074434,121.999999999998,-72.5734224782579));
#13485=CARTESIAN_POINT('Ctrl Pts',(-105.295732554092,121.999999999998,-73.2028454468363));
#13486=CARTESIAN_POINT('Ctrl Pts',(-105.184827334639,121.984047401261,-73.5660373895111));
#13487=CARTESIAN_POINT('Ctrl Pts',(-105.161274966764,121.956851469395,-73.936910595704));
#13488=CARTESIAN_POINT('Ctrl Pts',(-105.161274966764,121.956851469395,-73.936910595704));
#13489=CARTESIAN_POINT('Ctrl Pts',(-105.160208558995,121.955620087771,-73.9537030502982));
#13490=CARTESIAN_POINT('Ctrl Pts',(-105.159312222542,121.954368073319,-73.9705108670905));
#13491=CARTESIAN_POINT('Ctrl Pts',(-105.141806095166,121.923740934709,-74.3755987782653));
#13492=CARTESIAN_POINT('Ctrl Pts',(-105.220632281856,121.883764743458,-74.7699487335092));
#13493=CARTESIAN_POINT('Ctrl Pts',(-105.521158293664,121.805444228818,-75.5303372205339));
#13494=CARTESIAN_POINT('Ctrl Pts',(-105.789528120238,121.763409572459,-75.9328808434969));
#13495=CARTESIAN_POINT('Ctrl Pts',(-106.453707797634,121.708045140711,-76.628542676721));
#13496=CARTESIAN_POINT('Ctrl Pts',(-106.848809084286,121.694880858045,-76.9223501948628));
#13497=CARTESIAN_POINT('Ctrl Pts',(-107.691771010159,121.694880858045,-77.4090344896822));
#13498=CARTESIAN_POINT('Ctrl Pts',(-108.220065215752,121.712442638456,-77.6261028768581));
#13499=CARTESIAN_POINT('Ctrl Pts',(-109.312089805283,121.775514411454,-77.895062699818));
#13500=CARTESIAN_POINT('Ctrl Pts',(-109.875597099252,121.820378366244,-77.948009947617));
#13501=CARTESIAN_POINT('Ctrl Pts',(-110.764678189875,121.895265649918,-77.8679069906454));
#13502=CARTESIAN_POINT('Ctrl Pts',(-111.160729658472,121.930081208774,-77.7775411098295));
#13503=CARTESIAN_POINT('Ctrl Pts',(-111.678984353092,121.96968170959,-77.5193177005707));
#13504=CARTESIAN_POINT('Ctrl Pts',(-111.839559773292,121.980744602752,-77.4130886523666));
#13505=CARTESIAN_POINT('Ctrl Pts',(-112.11953636853,121.995916933756,-77.161529052004));
#13506=CARTESIAN_POINT('Ctrl Pts',(-112.238887146792,121.999999999998,-77.016140826053));
#13507=CARTESIAN_POINT('Ctrl Pts',(-112.425073184787,121.999999999998,-76.693657148586));
#13508=CARTESIAN_POINT('Ctrl Pts',(-112.491307692741,121.995916933756,-76.5176022296746));
#13509=CARTESIAN_POINT('Ctrl Pts',(-112.568812151847,121.980815574618,-76.1510781390455));
#13510=CARTESIAN_POINT('Ctrl Pts',(-112.580669535468,121.969889075075,-75.9607734026514));
#13511=CARTESIAN_POINT('Ctrl Pts',(-112.569378637745,121.956851469395,-75.7699408736867));
#13512=CARTESIAN_POINT('',(-101.043673435707,121.93955176967,-68.8916782754278));
#13513=CARTESIAN_POINT('',(-94.7826830987082,121.939551769669,-68.1687213841338));
#13514=CARTESIAN_POINT('Ctrl Pts',(-101.043673435707,121.93955176967,-68.8916782754277));
#13515=CARTESIAN_POINT('Ctrl Pts',(-101.030778440127,121.913761778509,-68.5765055229452));
#13516=CARTESIAN_POINT('Ctrl Pts',(-100.960164861362,121.882510881795,-68.2634583404383));
#13517=CARTESIAN_POINT('Ctrl Pts',(-100.712810634339,121.813417983957,-67.5935677254039));
#13518=CARTESIAN_POINT('Ctrl Pts',(-100.483220636953,121.771343589081,-67.2056047409378));
#13519=CARTESIAN_POINT('Ctrl Pts',(-99.9029587467504,121.711697111731,-66.5303819021385));
#13520=CARTESIAN_POINT('Ctrl Pts',(-99.5520623213409,121.694880858045,-66.2432484721442));
#13521=CARTESIAN_POINT('Ctrl Pts',(-99.1908428113955,121.694880858045,-66.0346982908408));
#13522=CARTESIAN_POINT('Ctrl Pts',(-98.8578333531796,121.694880858045,-65.8424351904971));
#13523=CARTESIAN_POINT('Ctrl Pts',(-98.4675142149001,121.709425126322,-65.6899158622252));
#13524=CARTESIAN_POINT('Ctrl Pts',(-97.6636618634519,121.766292452039,-65.5478256106297));
#13525=CARTESIAN_POINT('Ctrl Pts',(-97.2499629860219,121.808024204338,-65.5589567845263));
#13526=CARTESIAN_POINT('Ctrl Pts',(-96.532228635356,121.885750778307,-65.7270017969835));
#13527=CARTESIAN_POINT('Ctrl Pts',(-96.1806212553106,121.926229231586,-65.8836810953591));
#13528=CARTESIAN_POINT('Ctrl Pts',(-95.5755231979279,121.983802794611,-66.3313873276683));
#13529=CARTESIAN_POINT('Ctrl Pts',(-95.3217546974658,121.999999999998,-66.6221537056877));
#13530=CARTESIAN_POINT('Ctrl Pts',(-94.9650500672789,121.999999999998,-67.2399842484664));
#13531=CARTESIAN_POINT('Ctrl Pts',(-94.8401232475787,121.983802794611,-67.6051374055565));
#13532=CARTESIAN_POINT('Ctrl Pts',(-94.7903548426391,121.950162492739,-68.0421265757317));
#13533=CARTESIAN_POINT('Ctrl Pts',(-94.7854013049624,121.944988182178,-68.1054231196404));
#13534=CARTESIAN_POINT('Ctrl Pts',(-94.7826830987084,121.93955176967,-68.168721384132));
#13535=CARTESIAN_POINT('Ctrl Pts',(-94.7826830987083,121.93955176967,-68.168721384132));
#13536=CARTESIAN_POINT('Ctrl Pts',(-94.7692793143766,121.912744201006,-68.4808523287743));
#13537=CARTESIAN_POINT('Ctrl Pts',(-94.8123721828179,121.87944427626,-68.7931115535356));
#13538=CARTESIAN_POINT('Ctrl Pts',(-95.0083986686057,121.808024204338,-69.4414600707244));
#13539=CARTESIAN_POINT('Ctrl Pts',(-95.2056082279524,121.766292452039,-69.8052993950442));
#13540=CARTESIAN_POINT('Ctrl Pts',(-95.7305881711883,121.709425126322,-70.4304108264924));
#13541=CARTESIAN_POINT('Ctrl Pts',(-96.0578333531797,121.694880858045,-70.6921774516898));
#13542=CARTESIAN_POINT('Ctrl Pts',(-96.7520623213409,121.694880858045,-71.0929907333369));
#13543=CARTESIAN_POINT('Ctrl Pts',(-97.1761753786965,121.711697111731,-71.2533092368416));
#13544=CARTESIAN_POINT('Ctrl Pts',(-98.0510664554135,121.771343589081,-71.4182193552053));
#13545=CARTESIAN_POINT('Ctrl Pts',(-98.5018472543822,121.813417983957,-71.4230686331636));
#13546=CARTESIAN_POINT('Ctrl Pts',(-99.2682419576485,121.888653805311,-71.2916044625037));
#13547=CARTESIAN_POINT('Ctrl Pts',(-99.6421808158843,121.927100882661,-71.163309142685));
#13548=CARTESIAN_POINT('Ctrl Pts',(-100.289083992022,121.983258351228,-70.7579195346131));
#13549=CARTESIAN_POINT('Ctrl Pts',(-100.561342752554,121.999999999998,-70.4795670133904));
#13550=CARTESIAN_POINT('Ctrl Pts',(-100.92546201219,121.999999999998,-69.8488939556873));
#13551=CARTESIAN_POINT('Ctrl Pts',(-101.03039298651,121.983258351228,-69.4739346920516));
#13552=CARTESIAN_POINT('Ctrl Pts',(-101.046625787479,121.950260836241,-69.0256457187578));
#13553=CARTESIAN_POINT('Ctrl Pts',(-101.046412113711,121.945029125677,-68.9586156139657));
#13554=CARTESIAN_POINT('Ctrl Pts',(-101.043673435707,121.93955176967,-68.8916782754277));
#13555=CARTESIAN_POINT('',(-89.6457108608091,121.928269354306,-62.1822365876521));
#13556=CARTESIAN_POINT('',(-83.8969144629603,121.928269354306,-62.0126448588956));
#13557=CARTESIAN_POINT('Ctrl Pts',(-89.6457108608091,121.928269354306,-62.1822365876521));
#13558=CARTESIAN_POINT('Ctrl Pts',(-89.640048215299,121.903866743648,-61.9118469440624));
#13559=CARTESIAN_POINT('Ctrl Pts',(-89.5938110699338,121.875525701933,-61.6447310127997));
#13560=CARTESIAN_POINT('Ctrl Pts',(-89.4114212651875,121.810267922929,-61.0498367272997));
#13561=CARTESIAN_POINT('Ctrl Pts',(-89.2283577823594,121.76941928365,-60.6962570673076));
#13562=CARTESIAN_POINT('Ctrl Pts',(-88.7408793475757,121.711304602249,-60.0841026261431));
#13563=CARTESIAN_POINT('Ctrl Pts',(-88.4363138250625,121.694880858045,-59.8255680855737));
#13564=CARTESIAN_POINT('Ctrl Pts',(-88.11715467285,121.694880858045,-59.6413014631295));
#13565=CARTESIAN_POINT('Ctrl Pts',(-87.8077521236662,121.694880858045,-59.4626678180703));
#13566=CARTESIAN_POINT('Ctrl Pts',(-87.4431698769551,121.710493799957,-59.3305852473804));
#13567=CARTESIAN_POINT('Ctrl Pts',(-86.6945172380366,121.768237475725,-59.2263000150256));
#13568=CARTESIAN_POINT('Ctrl Pts',(-86.3103592215609,121.809531015002,-59.2542646021946));
#13569=CARTESIAN_POINT('Ctrl Pts',(-85.6299700128694,121.886577617489,-59.4387756069027));
#13570=CARTESIAN_POINT('Ctrl Pts',(-85.2887695763051,121.927161354661,-59.6051048904537));
#13571=CARTESIAN_POINT('Ctrl Pts',(-84.7006180249038,121.984260557561,-60.0622377416933));
#13572=CARTESIAN_POINT('Ctrl Pts',(-84.4534935750556,121.999999999998,-60.35291487129));
#13573=CARTESIAN_POINT('Ctrl Pts',(-84.1015994130934,121.999999999998,-60.9624134386954));
#13574=CARTESIAN_POINT('Ctrl Pts',(-83.9734278594876,121.98426055756,-61.3217680549585));
#13575=CARTESIAN_POINT('Ctrl Pts',(-83.9077720873625,121.947439165029,-61.7976287162892));
#13576=CARTESIAN_POINT('Ctrl Pts',(-83.8992173832946,121.938193561674,-61.9053402793198));
#13577=CARTESIAN_POINT('Ctrl Pts',(-83.8969144629603,121.928269354306,-62.0126448588956));
#13578=CARTESIAN_POINT('Ctrl Pts',(-83.8969144629603,121.928269354306,-62.0126448588956));
#13579=CARTESIAN_POINT('Ctrl Pts',(-83.8912689889189,121.903940742393,-62.2756957380355));
#13580=CARTESIAN_POINT('Ctrl Pts',(-83.9241062924374,121.875500673982,-62.5363189359234));
#13581=CARTESIAN_POINT('Ctrl Pts',(-84.0785731934348,121.809531015002,-63.1198313945313));
#13582=CARTESIAN_POINT('Ctrl Pts',(-84.246434158778,121.768237475725,-63.4665042894511));
#13583=CARTESIAN_POINT('Ctrl Pts',(-84.7110741386961,121.710493799957,-64.0627138771875));
#13584=CARTESIAN_POINT('Ctrl Pts',(-85.0077521236662,121.694880858045,-64.3124100792631));
#13585=CARTESIAN_POINT('Ctrl Pts',(-85.6363138250625,121.694880858045,-64.6753103467665));
#13586=CARTESIAN_POINT('Ctrl Pts',(-86.012494066208,121.711304602249,-64.8098045560952));
#13587=CARTESIAN_POINT('Ctrl Pts',(-86.7863745806878,121.76941928365,-64.9258960438327));
#13588=CARTESIAN_POINT('Ctrl Pts',(-87.1841152899164,121.810267922929,-64.907643840471));
#13589=CARTESIAN_POINT('Ctrl Pts',(-87.8886874328802,121.886091946244,-64.7455648365782));
#13590=CARTESIAN_POINT('Ctrl Pts',(-88.245336954858,121.9263037894,-64.5935914546221));
#13591=CARTESIAN_POINT('Ctrl Pts',(-88.8607180558249,121.983695909948,-64.1544777755007));
#13592=CARTESIAN_POINT('Ctrl Pts',(-89.1191660952628,121.999999999998,-63.866826235406));
#13593=CARTESIAN_POINT('Ctrl Pts',(-89.4775721811683,121.999999999998,-63.2460486848757));
#13594=CARTESIAN_POINT('Ctrl Pts',(-89.5974617026091,121.983695909948,-62.8784003471169));
#13595=CARTESIAN_POINT('Ctrl Pts',(-89.6440171485706,121.946889139357,-62.3958111209995));
#13596=CARTESIAN_POINT('Ctrl Pts',(-89.6479419658163,121.937884080627,-62.2887711900116));
#13597=CARTESIAN_POINT('Ctrl Pts',(-89.6457108608091,121.928269354306,-62.1822365876521));
#13598=CARTESIAN_POINT('',(-75.5607164801933,121.77184403287,-52.8249999999979));
#13599=CARTESIAN_POINT('',(-75.5607164801932,121.77184403287,-58.4249999999981));
#13600=CARTESIAN_POINT('Ctrl Pts',(-75.5607164801933,121.77184403287,-52.8249999999979));
#13601=CARTESIAN_POINT('Ctrl Pts',(-75.31087199813,121.795561855846,-52.8249999999979));
#13602=CARTESIAN_POINT('Ctrl Pts',(-75.0641712044988,121.822609441991,-52.8592756004775));
#13603=CARTESIAN_POINT('Ctrl Pts',(-74.4972946958141,121.886557224277,-53.0111697031877));
#13604=CARTESIAN_POINT('Ctrl Pts',(-74.1537701819123,121.927083062952,-53.1755443283788));
#13605=CARTESIAN_POINT('Ctrl Pts',(-73.561230066802,121.984194331231,-53.6296591429951));
#13606=CARTESIAN_POINT('Ctrl Pts',(-73.3122219315277,121.999999999998,-53.9195067988283));
#13607=CARTESIAN_POINT('Ctrl Pts',(-72.9594687676658,121.999999999998,-54.5304932011677));
#13608=CARTESIAN_POINT('Ctrl Pts',(-72.8329574021241,121.984194331231,-54.8910643999808));
#13609=CARTESIAN_POINT('Ctrl Pts',(-72.7359524939867,121.927083062952,-55.6312765997358));
#13610=CARTESIAN_POINT('Ctrl Pts',(-72.7653621497846,121.886557224277,-56.010964868193));
#13611=CARTESIAN_POINT('Ctrl Pts',(-72.9468930668116,121.810132271938,-56.6884474736823));
#13612=CARTESIAN_POINT('Ctrl Pts',(-73.1112681701126,121.769187929666,-57.0319552746733));
#13613=CARTESIAN_POINT('Ctrl Pts',(-73.5653642866542,121.711112887006,-57.6244722503148));
#13614=CARTESIAN_POINT('Ctrl Pts',(-73.855200110294,121.694880858045,-57.8734811721914));
#13615=CARTESIAN_POINT('Ctrl Pts',(-74.4662328500925,121.694880858045,-58.2262610889977));
#13616=CARTESIAN_POINT('Ctrl Pts',(-74.8267988140265,121.711112887006,-58.3527618142583));
#13617=CARTESIAN_POINT('Ctrl Pts',(-75.3177281966151,121.749631404864,-58.4170976637661));
#13618=CARTESIAN_POINT('Ctrl Pts',(-75.4395919608409,121.760345640413,-58.4249999999981));
#13619=CARTESIAN_POINT('Ctrl Pts',(-75.560716480193,121.77184403287,-58.4249999999981));
#13620=CARTESIAN_POINT('Ctrl Pts',(-75.560716480193,121.77184403287,-58.4249999999981));
#13621=CARTESIAN_POINT('Ctrl Pts',(-75.8105609622564,121.795561855846,-58.4249999999981));
#13622=CARTESIAN_POINT('Ctrl Pts',(-76.0572617558877,121.822609441991,-58.3907243995186));
#13623=CARTESIAN_POINT('Ctrl Pts',(-76.6241382645725,121.886557224277,-58.2388302968083));
#13624=CARTESIAN_POINT('Ctrl Pts',(-76.9676627784743,121.927083062952,-58.0744556716172));
#13625=CARTESIAN_POINT('Ctrl Pts',(-77.5602028935846,121.984194331231,-57.620340857001));
#13626=CARTESIAN_POINT('Ctrl Pts',(-77.8092110288589,121.999999999998,-57.3304932011678));
#13627=CARTESIAN_POINT('Ctrl Pts',(-78.1619641927208,121.999999999998,-56.7195067988283));
#13628=CARTESIAN_POINT('Ctrl Pts',(-78.2884755582626,121.984194331231,-56.3589356000152));
#13629=CARTESIAN_POINT('Ctrl Pts',(-78.3854804663999,121.927083062952,-55.6187234002602));
#13630=CARTESIAN_POINT('Ctrl Pts',(-78.356070810602,121.886557224277,-55.239035131803));
#13631=CARTESIAN_POINT('Ctrl Pts',(-78.174539893575,121.810132271938,-54.5615525263137));
#13632=CARTESIAN_POINT('Ctrl Pts',(-78.010164790274,121.769187929666,-54.2180447253227));
#13633=CARTESIAN_POINT('Ctrl Pts',(-77.5560686737324,121.711112887006,-53.6255277496812));
#13634=CARTESIAN_POINT('Ctrl Pts',(-77.2662328500926,121.694880858045,-53.3765188278046));
#13635=CARTESIAN_POINT('Ctrl Pts',(-76.9607164801934,121.694880858045,-53.2001288694015));
#13636=CARTESIAN_POINT('Ctrl Pts',(-76.6552001102941,121.694880858045,-53.0237389109983));
#13637=CARTESIAN_POINT('Ctrl Pts',(-76.2946341463601,121.711112887006,-52.8972381857377));
#13638=CARTESIAN_POINT('Ctrl Pts',(-75.8037047637714,121.749631404864,-52.8329023362299));
#13639=CARTESIAN_POINT('Ctrl Pts',(-75.6818409995455,121.760345640413,-52.8249999999979));
#13640=CARTESIAN_POINT('Ctrl Pts',(-75.5607164801933,121.77184403287,-52.8249999999979));
#13641=CARTESIAN_POINT('Origin',(-115.614391405224,109.,-78.7499999999976));
#13642=CARTESIAN_POINT('Origin',(-111.692877174869,125.221825406948,-76.4859127034721));
#13643=CARTESIAN_POINT('',(-109.047125863805,127.513113254426,-76.4859127034721));
#13644=CARTESIAN_POINT('Origin',(-111.692877174869,125.221825406948,-76.4859127034721));
#13645=CARTESIAN_POINT('',(-109.576276126018,127.054855684931,-76.4859127034722));
#13646=CARTESIAN_POINT('Origin',(-111.692877174869,125.221825406948,-76.4859127034722));
#13647=CARTESIAN_POINT('Origin',(-111.692877174869,125.221825406948,-76.4859127034721));
#13648=CARTESIAN_POINT('',(-109.047125863805,127.513113254426,-76.4859127034721));
#13649=CARTESIAN_POINT('Origin',(-75.5607164801933,112.,-55.624999999998));
#13650=CARTESIAN_POINT('',(-75.5607164801933,112.,-58.4249999999981));
#13651=CARTESIAN_POINT('Origin',(-84.3932587967998,111.68028146752,-60.7244706841197));
#13652=CARTESIAN_POINT('',(-81.6657313432502,112.313206415782,-60.7244706841197));
#13653=CARTESIAN_POINT('Origin',(-93.3501356426365,112.813466520527,-65.8957259421618));
#13654=CARTESIAN_POINT('',(-90.8457395078369,114.065664587927,-65.8957259421618));
#13655=CARTESIAN_POINT('Origin',(-103.119663075128,115.322330470337,-71.5361652351663));
#13656=CARTESIAN_POINT('',(-101.003062026277,117.155360748319,-71.5361652351663));
#13657=CARTESIAN_POINT('Origin',(-84.2209705180366,98.999999999999,-40.6249999999996));
#13658=CARTESIAN_POINT('',(-86.8190467293899,101.999999999999,-40.1249999999996));
#13659=CARTESIAN_POINT('Origin',(-84.2209705180366,98.999999999999,-40.6249999999996));
#13660=CARTESIAN_POINT('',(-86.4942872029708,101.624999999999,-40.1874999999995));
#13661=CARTESIAN_POINT('Origin',(-84.2209705180366,98.999999999999,-40.6249999999996));
#13662=CARTESIAN_POINT('Origin',(-26.1968246264604,166.000512499998,-141.125768750001));
#13663=CARTESIAN_POINT('',(-28.7949008378137,169.000512499998,-140.625768750001));
#13664=CARTESIAN_POINT('',(-80.5957703324788,98.5672184524782,-46.904030908994));
#13665=CARTESIAN_POINT('',(-80.5957703324788,98.567218452478,-46.9040309089941));
#13666=CARTESIAN_POINT('',(-82.595770332479,105.495421682753,-43.4399292938557));
#13667=CARTESIAN_POINT('Ctrl Pts',(-80.5957703324787,98.5672184524781,-46.9040309089941));
#13668=CARTESIAN_POINT('Ctrl Pts',(-80.1583076046396,98.5672184524781,-46.6514616853158));
#13669=CARTESIAN_POINT('Ctrl Pts',(-79.731847375509,98.6399471087077,-46.316319579711));
#13670=CARTESIAN_POINT('Ctrl Pts',(-79.0280064685973,98.9402745490956,-45.5660699284182));
#13671=CARTESIAN_POINT('Ctrl Pts',(-78.7496249554672,99.168633673537,-45.1522067177974));
#13672=CARTESIAN_POINT('Ctrl Pts',(-78.3748022679429,99.7108672272503,-44.3867423304201));
#13673=CARTESIAN_POINT('Ctrl Pts',(-78.2527827584179,100.061688880156,-43.983215927173));
#13674=CARTESIAN_POINT('Ctrl Pts',(-78.1901153330479,100.862134488935,-43.2736771449321));
#13675=CARTESIAN_POINT('Ctrl Pts',(-78.2490409596484,101.312629171298,-42.9686854143502));
#13676=CARTESIAN_POINT('Ctrl Pts',(-78.5015571253347,102.1873708287,-42.531314585649));
#13677=CARTESIAN_POINT('Ctrl Pts',(-78.7110997683144,102.666877512603,-42.3713056330979));
#13678=CARTESIAN_POINT('Ctrl Pts',(-79.2661565338858,103.572118612493,-42.2280010610046));
#13679=CARTESIAN_POINT('Ctrl Pts',(-79.6121998656049,103.997338243878,-42.2435068221059));
#13680=CARTESIAN_POINT('Ctrl Pts',(-80.340691634629,104.680250326612,-42.3963983912593));
#13681=CARTESIAN_POINT('Ctrl Pts',(-80.7727618736163,104.984284565641,-42.5440649201448));
#13682=CARTESIAN_POINT('Ctrl Pts',(-81.6811020778789,105.3923634715,-42.9401113983139));
#13683=CARTESIAN_POINT('Ctrl Pts',(-82.15830760464,105.495421682753,-43.1873600701774));
#13684=CARTESIAN_POINT('Ctrl Pts',(-82.595770332479,105.495421682753,-43.4399292938557));
#13685=CARTESIAN_POINT('',(-82.595770332479,105.495421682753,-43.4399292938557));
#13686=CARTESIAN_POINT('Origin',(-66.9004624423481,99.0000000000011,-70.6249999999998));
#13687=CARTESIAN_POINT('',(-69.4985386537014,96.000000000001,-70.1249999999998));
#13688=CARTESIAN_POINT('Origin',(-66.9004624423481,99.0000000000011,-70.6249999999998));
#13689=CARTESIAN_POINT('',(-69.1737791272823,96.375000000001,-70.1874999999998));
#13690=CARTESIAN_POINT('Origin',(-66.9004624423481,99.0000000000011,-70.6249999999998));
#13691=CARTESIAN_POINT('Origin',(-124.924608333924,166.000512500002,29.8757687500004));
#13692=CARTESIAN_POINT('',(-127.522684545277,163.000512500001,30.3757687500005));
#13693=CARTESIAN_POINT('',(-68.5256626279059,105.495421682756,-67.8100707061432));
#13694=CARTESIAN_POINT('',(-68.5256626279059,105.495421682756,-67.8100707061433));
#13695=CARTESIAN_POINT('',(-70.5256626279056,98.5672184524799,-64.3459690910059));
#13696=CARTESIAN_POINT('Ctrl Pts',(-68.5256626279059,105.495421682756,-67.8100707061432));
#13697=CARTESIAN_POINT('Ctrl Pts',(-68.0881999000668,105.495421682756,-67.5575014824649));
#13698=CARTESIAN_POINT('Ctrl Pts',(-67.6354735058005,105.392363471503,-67.2678537093952));
#13699=CARTESIAN_POINT('Ctrl Pts',(-66.8383170924954,104.984284565643,-66.6792312563097));
#13700=CARTESIAN_POINT('Ctrl Pts',(-66.4943990076982,104.680250326615,-66.3788807175702));
#13701=CARTESIAN_POINT('Ctrl Pts',(-65.9977451402748,103.99733824388,-65.8244341237244));
#13702=CARTESIAN_POINT('Ctrl Pts',(-65.8112950913965,103.572118612495,-65.5325046881962));
#13703=CARTESIAN_POINT('Ctrl Pts',(-65.657872108522,102.666877512605,-64.9801591426223));
#13704=CARTESIAN_POINT('Ctrl Pts',(-65.6916726047743,102.187370828702,-64.7186854143503));
#13705=CARTESIAN_POINT('Ctrl Pts',(-65.9441887704605,101.3126291713,-64.2813145856493));
#13706=CARTESIAN_POINT('Ctrl Pts',(-66.1788565437883,100.862134488937,-64.0777876307885));
#13707=CARTESIAN_POINT('Ctrl Pts',(-66.8246688668641,100.061688880158,-63.7772898220283));
#13708=CARTESIAN_POINT('Ctrl Pts',(-67.2351427379364,99.7108672272523,-63.6811986154108));
#13709=CARTESIAN_POINT('Ctrl Pts',(-68.0854656868595,99.1686336735389,-63.623072391033));
#13710=CARTESIAN_POINT('Ctrl Pts',(-68.5830724975138,98.9402745490975,-63.6572262480373));
#13711=CARTESIAN_POINT('Ctrl Pts',(-69.5847282081697,98.6399471087095,-63.8916455279991));
#13712=CARTESIAN_POINT('Ctrl Pts',(-70.0881999000665,98.5672184524799,-64.0933998673275));
#13713=CARTESIAN_POINT('Ctrl Pts',(-70.5256626279056,98.5672184524799,-64.3459690910059));
#13714=CARTESIAN_POINT('',(-70.5256626279056,98.5672184524799,-64.3459690910059));
#13715=CARTESIAN_POINT('Origin',(-96.4746890553668,99.4494897427822,-48.5986671816671));
#13716=CARTESIAN_POINT('',(-94.430917460329,100.684620539947,-45.3897032396429));
#13717=CARTESIAN_POINT('Origin',(-96.4746890553668,99.4494897427822,-48.5986671816671));
#13718=CARTESIAN_POINT('',(-94.6863889097089,100.530229190302,-45.7908237323958));
#13719=CARTESIAN_POINT('Origin',(-96.4746890553669,99.4494897427822,-48.598667181667));
#13720=CARTESIAN_POINT('Origin',(41.8109368646032,203.413715679656,-176.687875705469));
#13721=CARTESIAN_POINT('',(43.8547084596409,204.648846476821,-173.478911763445));
#13722=CARTESIAN_POINT('Origin',(-79.9327200516597,99.449489742784,-77.250197953318));
#13723=CARTESIAN_POINT('',(-77.1059069082159,97.3101804481012,-75.3975017575705));
#13724=CARTESIAN_POINT('Origin',(-79.9327200516597,99.449489742784,-77.250197953318));
#13725=CARTESIAN_POINT('',(-77.4592585511463,97.5775941099365,-75.629088782039));
#13726=CARTESIAN_POINT('Origin',(-79.9327200516597,99.4494897427839,-77.250197953318));
#13727=CARTESIAN_POINT('Origin',(-121.718415623925,203.413715679661,106.553271333508));
#13728=CARTESIAN_POINT('',(-118.891602480482,201.274406384978,108.405967529256));
#13729=CARTESIAN_POINT('Origin',(-108.737631016432,99.7320508075681,-56.2438021535162));
#13730=CARTESIAN_POINT('',(-107.276159708174,100.386816955051,-52.5783713592919));
#13731=CARTESIAN_POINT('Origin',(-108.737631016432,99.7320508075681,-56.2438021535162));
#13732=CARTESIAN_POINT('',(-107.458843621706,100.304971186616,-53.03655020857));
#13733=CARTESIAN_POINT('Origin',(-108.737631016432,99.732050807568,-56.2438021535162));
#13734=CARTESIAN_POINT('Origin',(125.171333134686,225.083486900949,-171.899270921774));
#13735=CARTESIAN_POINT('',(126.632804442944,225.738253048432,-168.23384012755));
#13736=CARTESIAN_POINT('Origin',(-92.6850721331748,99.7320508075696,-84.0476497308099));
#13737=CARTESIAN_POINT('',(-89.6744074864335,97.2884302780867,-83.0655005095853));
#13738=CARTESIAN_POINT('Origin',(-92.6850721331748,99.7320508075696,-84.0476497308099));
#13739=CARTESIAN_POINT('',(-90.0507405672762,97.5938828442721,-83.1882691622385));
#13740=CARTESIAN_POINT('Origin',(-92.6850721331748,99.7320508075696,-84.0476497308099));
#13741=CARTESIAN_POINT('Origin',(-75.8911640975186,225.083486900956,176.351189781088));
#13742=CARTESIAN_POINT('',(-72.8804994507773,222.639866371473,177.333339002313));
#13743=CARTESIAN_POINT('Origin',(-121.472809584586,99.8284271247455,-63.7892135623721));
#13744=CARTESIAN_POINT('',(-120.716880638568,99.8284271247455,-59.8612915381242));
#13745=CARTESIAN_POINT('Origin',(-121.472809584586,99.8284271247455,-63.7892135623721));
#13746=CARTESIAN_POINT('',(-120.81137175682,99.8284271247455,-60.3522817911552));
#13747=CARTESIAN_POINT('Origin',(-121.472809584586,99.8284271247455,-63.7892135623721));
#13748=CARTESIAN_POINT('Origin',(201.051502502506,223.968092727195,-125.859046363603));
#13749=CARTESIAN_POINT('',(201.807431448525,223.968092727195,-121.931124339356));
#13750=CARTESIAN_POINT('Origin',(-105.587179379326,99.8284271247468,-91.303932188134));
#13751=CARTESIAN_POINT('',(-102.563463595252,97.2098124419149,-91.303932188134));
#13752=CARTESIAN_POINT('Origin',(-105.587179379326,99.8284271247468,-91.303932188134));
#13753=CARTESIAN_POINT('',(-102.941428068262,97.5371392772689,-91.303932188134));
#13754=CARTESIAN_POINT('Origin',(-105.587179379326,99.8284271247468,-91.303932188134));
#13755=CARTESIAN_POINT('Origin',(1.92092464970915,223.968092727204,219.045231817999));
#13756=CARTESIAN_POINT('',(4.94464043378298,221.349478044372,219.045231817999));
#13757=CARTESIAN_POINT('Origin',(-74.2616783745156,107.500000000001,-57.8749999999998));
#13758=CARTESIAN_POINT('',(-70.018153895972,98.4000000000012,-68.0249999999999));
#13759=CARTESIAN_POINT('',(-76.080331722463,105.400000000001,-57.5249999999998));
#13760=CARTESIAN_POINT('Origin',(-68.1995005480246,100.500000000001,-68.3749999999999));
#13761=CARTESIAN_POINT('Origin',(-76.8597545858689,107.499999999999,-53.3749999999998));
#13762=CARTESIAN_POINT('',(-84.7405857603073,102.599999999999,-42.5249999999996));
#13763=CARTESIAN_POINT('',(-78.6784079338163,109.599999999999,-53.0249999999997));
#13764=CARTESIAN_POINT('Origin',(-82.9219324123599,100.499999999999,-42.8749999999997));
#13765=CARTESIAN_POINT('Origin',(-83.2326628767165,107.659859266241,-62.734681784761));
#13766=CARTESIAN_POINT('',(-78.5362937027295,99.4008619759398,-73.3917489394908));
#13767=CARTESIAN_POINT('',(-81.2538936763059,106.162342759963,-61.4377944477378));
#13768=CARTESIAN_POINT('Origin',(-80.5150629031402,100.898378482218,-74.6886362765139));
#13769=CARTESIAN_POINT('Origin',(-85.5538547168813,107.659859266239,-58.7142595834813));
#13770=CARTESIAN_POINT('',(-93.1168428791077,101.762970040231,-48.1374969637468));
#13771=CARTESIAN_POINT('',(-84.1232146003549,108.524450824255,-56.4679848240644));
#13772=CARTESIAN_POINT('Origin',(-94.5474829956341,100.898378482216,-50.3837717231637));
#13773=CARTESIAN_POINT('Origin',(-91.6988562010068,107.093266739737,-68.7558258325585));
#13774=CARTESIAN_POINT('',(-90.4035687747792,99.3205545426085,-80.661588117438));
#13775=CARTESIAN_POINT('',(-89.5913909482879,105.3827323691,-68.0683213777014));
#13776=CARTESIAN_POINT('Origin',(-92.511034027498,101.031088913246,-81.3490925722951));
#13777=CARTESIAN_POINT('Origin',(-95.0014150842646,107.093266739736,-63.0356260517679));
#13778=CARTESIAN_POINT('',(-105.290562994975,101.489425216483,-54.8765577560743));
#13779=CARTESIAN_POINT('',(-93.9783851684838,107.551603042974,-60.469824495811));
#13780=CARTESIAN_POINT('Origin',(-106.313592910756,101.031088913245,-57.4423593120313));
#13781=CARTESIAN_POINT('Origin',(-100.382013675912,105.838834764833,-76.2779130879201));
#13782=CARTESIAN_POINT('',(-102.552019676931,99.0560570185445,-88.6522817586846));
#13783=CARTESIAN_POINT('',(-98.2654126270599,104.00580448685,-76.2779130879202));
#13784=CARTESIAN_POINT('Origin',(-104.668620725782,100.889087296527,-88.6522817586846));
#13785=CARTESIAN_POINT('Origin',(-105.857312474343,105.838834764831,-66.7944173824152));
#13786=CARTESIAN_POINT('',(-118.187983361742,100.889087296525,-61.5699982312887));
#13787=CARTESIAN_POINT('',(-105.328162212131,105.838834764831,-64.0448719654417));
#13788=CARTESIAN_POINT('Origin',(-118.717133623955,100.889087296525,-64.3195436482622));
#13789=CARTESIAN_POINT('Origin',(-82.9219324123599,100.499999999999,-42.8749999999996));
#13790=CARTESIAN_POINT('',(-85.1952490972941,103.124999999999,-42.4374999999996));
#13791=CARTESIAN_POINT('Origin',(-82.9219324123599,100.499999999999,-42.8749999999996));
#13792=CARTESIAN_POINT('Origin',(-82.9219324123599,100.499999999999,-42.8749999999996));
#13793=CARTESIAN_POINT('',(-85.1952490972941,103.124999999999,-42.4374999999996));
#13794=CARTESIAN_POINT('Origin',(-68.1995005480247,100.500000000001,-68.3749999999998));
#13795=CARTESIAN_POINT('',(-70.4728172329589,97.875000000001,-67.9374999999998));
#13796=CARTESIAN_POINT('Origin',(-68.1995005480247,100.500000000001,-68.3749999999998));
#13797=CARTESIAN_POINT('Origin',(-68.1995005480247,100.500000000001,-68.3749999999998));
#13798=CARTESIAN_POINT('',(-70.4728172329589,97.875000000001,-67.9374999999998));
#13799=CARTESIAN_POINT('Origin',(-94.5474829956341,100.898378482216,-50.3837717231636));
#13800=CARTESIAN_POINT('',(-92.7591828499761,101.979117929735,-47.5759282738925));
#13801=CARTESIAN_POINT('Origin',(-94.5474829956341,100.898378482216,-50.3837717231636));
#13802=CARTESIAN_POINT('Origin',(-94.5474829956341,100.898378482216,-50.3837717231636));
#13803=CARTESIAN_POINT('',(-92.7591828499761,101.979117929735,-47.5759282738925));
#13804=CARTESIAN_POINT('Origin',(-80.5150629031403,100.898378482218,-74.6886362765138));
#13805=CARTESIAN_POINT('',(-78.041601402627,99.0264828493701,-73.0675271052348));
#13806=CARTESIAN_POINT('Origin',(-80.5150629031403,100.898378482218,-74.6886362765138));
#13807=CARTESIAN_POINT('Origin',(-80.5150629031403,100.898378482218,-74.6886362765138));
#13808=CARTESIAN_POINT('',(-78.041601402627,99.0264828493701,-73.0675271052348));
#13809=CARTESIAN_POINT('Origin',(-106.313592910756,101.031088913245,-57.4423593120312));
#13810=CARTESIAN_POINT('',(-105.03480551603,101.604009292292,-54.235107367085));
#13811=CARTESIAN_POINT('Origin',(-106.313592910756,101.031088913245,-57.4423593120312));
#13812=CARTESIAN_POINT('Origin',(-106.313592910756,101.031088913245,-57.4423593120312));
#13813=CARTESIAN_POINT('',(-105.03480551603,101.604009292292,-54.235107367085));
#13814=CARTESIAN_POINT('Origin',(-92.5110340274981,101.031088913246,-81.349092572295));
#13815=CARTESIAN_POINT('',(-89.8767024615995,98.8929209499488,-80.4897120037236));
#13816=CARTESIAN_POINT('Origin',(-92.5110340274981,101.031088913246,-81.349092572295));
#13817=CARTESIAN_POINT('Origin',(-92.5110340274981,101.031088913246,-81.349092572295));
#13818=CARTESIAN_POINT('',(-89.8767024615995,98.8929209499488,-80.4897120037236));
#13819=CARTESIAN_POINT('Origin',(-118.717133623955,100.889087296525,-64.319543648262));
#13820=CARTESIAN_POINT('',(-118.055695796189,100.889087296525,-60.8826118770452));
#13821=CARTESIAN_POINT('Origin',(-118.717133623955,100.889087296525,-64.319543648262));
#13822=CARTESIAN_POINT('Origin',(-118.717133623955,100.889087296525,-64.319543648262));
#13823=CARTESIAN_POINT('',(-118.055695796189,100.889087296525,-60.8826118770452));
#13824=CARTESIAN_POINT('Origin',(-104.668620725782,100.889087296527,-88.6522817586845));
#13825=CARTESIAN_POINT('',(-102.022869414718,98.5977994490487,-88.6522817586845));
#13826=CARTESIAN_POINT('Origin',(-104.668620725782,100.889087296527,-88.6522817586845));
#13827=CARTESIAN_POINT('Origin',(-104.668620725782,100.889087296527,-88.6522817586845));
#13828=CARTESIAN_POINT('',(-102.022869414718,98.5977994490487,-88.6522817586845));
#13829=CARTESIAN_POINT('Origin',(-125.268934230709,90.999,-76.5975199760558));
#13830=CARTESIAN_POINT('',(-122.424179917669,121.863728726179,-74.9551003076436));
#13831=CARTESIAN_POINT('Origin',(-118.577560436093,90.999,-88.1873193607661));
#13832=CARTESIAN_POINT('',(-115.732806123053,121.863728726179,-86.5448996923539));
#13833=CARTESIAN_POINT('Origin',(-115.529994481957,90.999,-74.0824712601139));
#13834=CARTESIAN_POINT('',(-115.529994481957,122.937359864766,-74.0824712601139));
#13835=CARTESIAN_POINT('',(-115.529994481957,122.937359864766,-74.0824712601139));
#13836=CARTESIAN_POINT('',(-115.529994481957,122.937359864766,-74.082471260114));
#13837=CARTESIAN_POINT('Origin',(-111.529994481957,90.999,-81.0106744903897));
#13838=CARTESIAN_POINT('',(-111.529994481957,122.937359864767,-81.0106744903897));
#13839=CARTESIAN_POINT('',(-111.529994481957,122.937359864767,-81.0106744903897));
#13840=CARTESIAN_POINT('',(-111.529994481957,122.937359864767,-81.0106744903897));
#13841=CARTESIAN_POINT('Ctrl Pts',(-111.529994481957,122.930969193824,-81.0106744903897));
#13842=CARTESIAN_POINT('Ctrl Pts',(-111.529994481957,124.224440992555,-81.0106744903897));
#13843=CARTESIAN_POINT('Ctrl Pts',(-111.850631939497,122.930969193824,-81.1957946128129));
#13844=CARTESIAN_POINT('Ctrl Pts',(-111.850631939497,124.224440992555,-81.1957946128129));
#13845=CARTESIAN_POINT('Ctrl Pts',(-112.595893637265,122.930969193824,-81.3855792709696));
#13846=CARTESIAN_POINT('Ctrl Pts',(-112.595893637265,124.224440992555,-81.3855792709696));
#13847=CARTESIAN_POINT('Ctrl Pts',(-113.856111715799,122.930969193824,-81.0858699693662));
#13848=CARTESIAN_POINT('Ctrl Pts',(-113.856111715799,124.224440992555,-81.0858699693662));
#13849=CARTESIAN_POINT('Ctrl Pts',(-115.066649862454,122.930969193824,-80.2473165597762));
#13850=CARTESIAN_POINT('Ctrl Pts',(-115.066649862454,124.224440992555,-80.2473165597762));
#13851=CARTESIAN_POINT('Ctrl Pts',(-116.043255168468,122.930969193824,-78.9976046091529));
#13852=CARTESIAN_POINT('Ctrl Pts',(-116.043255168468,124.224440992555,-78.9976046091529));
#13853=CARTESIAN_POINT('Ctrl Pts',(-116.637234812114,122.930969193824,-77.5269836293621));
#13854=CARTESIAN_POINT('Ctrl Pts',(-116.637234812114,124.224440992555,-77.5269836293621));
#13855=CARTESIAN_POINT('Ctrl Pts',(-116.758174293921,122.930969193824,-76.0593501373141));
#13856=CARTESIAN_POINT('Ctrl Pts',(-116.758174293921,124.224440992555,-76.0593501373141));
#13857=CARTESIAN_POINT('Ctrl Pts',(-116.387621123593,122.930969193824,-74.8181146161938));
#13858=CARTESIAN_POINT('Ctrl Pts',(-116.387621123593,124.224440992555,-74.8181146161938));
#13859=CARTESIAN_POINT('Ctrl Pts',(-115.850631939497,122.930969193824,-74.2675913825374));
#13860=CARTESIAN_POINT('Ctrl Pts',(-115.850631939497,124.224440992555,-74.2675913825374));
#13861=CARTESIAN_POINT('Ctrl Pts',(-115.529994481957,122.930969193824,-74.0824712601142));
#13862=CARTESIAN_POINT('Ctrl Pts',(-115.529994481957,124.224440992555,-74.0824712601142));
#13863=CARTESIAN_POINT('Ctrl Pts',(-111.529994481957,122.937359864767,-81.0106744903897));
#13864=CARTESIAN_POINT('Ctrl Pts',(-111.655985564703,122.937359864767,-81.0834154759286));
#13865=CARTESIAN_POINT('Ctrl Pts',(-111.789124566157,122.941999166342,-81.1417276437762));
#13866=CARTESIAN_POINT('Ctrl Pts',(-112.132055648316,122.963800802529,-81.2508717728567));
#13867=CARTESIAN_POINT('Ctrl Pts',(-112.344262065112,122.985642902608,-81.2836304965519));
#13868=CARTESIAN_POINT('Ctrl Pts',(-112.890185001658,123.055781639719,-81.2942385303482));
#13869=CARTESIAN_POINT('Ctrl Pts',(-113.222304091371,123.111288356191,-81.2310605511146));
#13870=CARTESIAN_POINT('Ctrl Pts',(-114.040071204807,123.254369388729,-80.9469153854904));
#13871=CARTESIAN_POINT('Ctrl Pts',(-114.507617463249,123.341916036999,-80.64733737895));
#13872=CARTESIAN_POINT('Ctrl Pts',(-115.174813131733,123.441390970383,-80.050767705693));
#13873=CARTESIAN_POINT('Ctrl Pts',(-115.415868442681,123.470261290121,-79.7826739036937));
#13874=CARTESIAN_POINT('Ctrl Pts',(-115.755003463233,123.495239476746,-79.3250674771333));
#13875=CARTESIAN_POINT('Ctrl Pts',(-115.872462661464,123.49998997396,-79.1461011463315));
#13876=CARTESIAN_POINT('Ctrl Pts',(-116.085775238015,123.500009989414,-78.7767368883965));
#13877=CARTESIAN_POINT('Ctrl Pts',(-116.182038306449,123.495284034831,-78.5856508621904));
#13878=CARTESIAN_POINT('Ctrl Pts',(-116.408570505306,123.47040914673,-78.0640352851986));
#13879=CARTESIAN_POINT('Ctrl Pts',(-116.52014584973,123.4416707474,-77.7220494143149));
#13880=CARTESIAN_POINT('Ctrl Pts',(-116.700435952419,123.344280060835,-76.8627043141552));
#13881=CARTESIAN_POINT('Ctrl Pts',(-116.72827833538,123.260349185246,-76.3253510567926));
#13882=CARTESIAN_POINT('Ctrl Pts',(-116.580959608512,123.119417363555,-75.4852207472909));
#13883=CARTESIAN_POINT('Ctrl Pts',(-116.473976785389,123.063000944788,-75.16186977102));
#13884=CARTESIAN_POINT('Ctrl Pts',(-116.194331351315,122.989309527258,-74.6783741194887));
#13885=CARTESIAN_POINT('Ctrl Pts',(-116.055391044604,122.965592809847,-74.5005585112936));
#13886=CARTESIAN_POINT('Ctrl Pts',(-115.831958999688,122.946686478982,-74.2944546113625));
#13887=CARTESIAN_POINT('Ctrl Pts',(-115.771332129154,122.942999951482,-74.2445494425702));
#13888=CARTESIAN_POINT('Ctrl Pts',(-115.650653287831,122.938455031077,-74.1565333304243));
#13889=CARTESIAN_POINT('Ctrl Pts',(-115.591330433288,122.937359864766,-74.1178835881261));
#13890=CARTESIAN_POINT('Ctrl Pts',(-115.529994481957,122.937359864766,-74.0824712601142));
#13891=CARTESIAN_POINT('Origin',(-119.078493020361,109.,-80.7499999999988));
#13892=CARTESIAN_POINT('Origin',(-141.995606772677,139.904097174214,-47.6260732918001));
#13893=CARTESIAN_POINT('',(-111.835491639576,108.363035329266,-93.2952463908106));
#13894=CARTESIAN_POINT('Origin',(-145.341293669985,128.314297789504,-41.8311735994448));
#13895=CARTESIAN_POINT('',(-115.181178536884,96.7732359445553,-87.5003466984555));
#13896=CARTESIAN_POINT('Origin',(-134.275197369886,137.573299096998,-41.6148274600336));
#13897=CARTESIAN_POINT('',(-106.49494062967,105.495421682756,-89.7316435813967));
#13898=CARTESIAN_POINT('',(-106.49494062967,105.495421682756,-89.7316435813967));
#13899=CARTESIAN_POINT('',(-106.49494062967,105.495421682756,-89.7316435813966));
#13900=CARTESIAN_POINT('Origin',(-136.275197369886,130.645095866722,-38.1507258448956));
#13901=CARTESIAN_POINT('',(-108.494940629669,98.5672184524796,-86.2675419662591));
#13902=CARTESIAN_POINT('',(-108.494940629669,98.5672184524796,-86.2675419662591));
#13903=CARTESIAN_POINT('',(-108.494940629669,98.5672184524797,-86.2675419662591));
#13904=CARTESIAN_POINT('Ctrl Pts',(-108.497707871361,98.5704137879512,-86.2627489630519));
#13905=CARTESIAN_POINT('Ctrl Pts',(-107.937618152971,97.9236778885854,-87.2328528121005));
#13906=CARTESIAN_POINT('Ctrl Pts',(-108.818345328902,98.5704137879512,-86.4478690854752));
#13907=CARTESIAN_POINT('Ctrl Pts',(-108.258255610512,97.9236778885854,-87.4179729345238));
#13908=CARTESIAN_POINT('Ctrl Pts',(-109.407402641416,98.750783075701,-86.9082076752565));
#13909=CARTESIAN_POINT('Ctrl Pts',(-108.847312923026,98.1040471763352,-87.8783115243051));
#13910=CARTESIAN_POINT('Ctrl Pts',(-110.000372038795,99.5212554870629,-87.7642069906961));
#13911=CARTESIAN_POINT('Ctrl Pts',(-109.440282320405,98.8745195876971,-88.7343108397447));
#13912=CARTESIAN_POINT('Ctrl Pts',(-110.212301964103,100.674348937882,-88.6552937573345));
#13913=CARTESIAN_POINT('Ctrl Pts',(-109.652212245713,100.027613038516,-89.6253976063831));
#13914=CARTESIAN_POINT('Ctrl Pts',(-110.010968557873,102.034515403089,-89.4458315045219));
#13915=CARTESIAN_POINT('Ctrl Pts',(-109.450878839483,101.387779503723,-90.4159353535705));
#13916=CARTESIAN_POINT('Ctrl Pts',(-109.427009489273,103.394681868296,-90.0154602225416));
#13917=CARTESIAN_POINT('Ctrl Pts',(-108.866919770883,102.74794596893,-90.9855640715902));
#13918=CARTESIAN_POINT('Ctrl Pts',(-108.549340749734,104.547775319115,-90.2774669067221));
#13919=CARTESIAN_POINT('Ctrl Pts',(-107.989251031344,103.901039419749,-91.2475707557707));
#13920=CARTESIAN_POINT('Ctrl Pts',(-107.511538898252,105.318247730477,-90.1919400026446));
#13921=CARTESIAN_POINT('Ctrl Pts',(-106.951449179862,104.671511831111,-91.1620438516932));
#13922=CARTESIAN_POINT('Ctrl Pts',(-106.818345328902,105.498617018227,-89.9119707006131));
#13923=CARTESIAN_POINT('Ctrl Pts',(-106.258255610512,104.851881118861,-90.8820745496617));
#13924=CARTESIAN_POINT('Ctrl Pts',(-106.497707871361,105.498617018227,-89.7268505781898));
#13925=CARTESIAN_POINT('Ctrl Pts',(-105.937618152971,104.851881118861,-90.6969544272384));
#13926=CARTESIAN_POINT('Ctrl Pts',(-108.494940629669,98.5672184524797,-86.2675419662592));
#13927=CARTESIAN_POINT('Ctrl Pts',(-108.620931712415,98.5672184524797,-86.3402829517981));
#13928=CARTESIAN_POINT('Ctrl Pts',(-108.740009575843,98.5788155545531,-86.4229497251191));
#13929=CARTESIAN_POINT('Ctrl Pts',(-109.015792308145,98.634550154098,-86.6483982077968));
#13930=CARTESIAN_POINT('Ctrl Pts',(-109.160240827059,98.6909481351825,-86.7985170532378));
#13931=CARTESIAN_POINT('Ctrl Pts',(-109.477961818401,98.884314307059,-87.2043824505149));
#13932=CARTESIAN_POINT('Ctrl Pts',(-109.620465834967,99.047756217635,-87.4696274118531));
#13933=CARTESIAN_POINT('Ctrl Pts',(-109.88505667753,99.5434281228911,-88.1436116529208));
#13934=CARTESIAN_POINT('Ctrl Pts',(-109.944782655288,99.9267917722889,-88.5503990928816));
#13935=CARTESIAN_POINT('Ctrl Pts',(-109.931222669289,100.613385759641,-89.132932800729));
#13936=CARTESIAN_POINT('Ctrl Pts',(-109.895248991132,100.904400962771,-89.3446672830305));
#13937=CARTESIAN_POINT('Ctrl Pts',(-109.799168414145,101.381966460934,-89.6408763836526));
#13938=CARTESIAN_POINT('Ctrl Pts',(-109.754281345734,101.564677285217,-89.7431020350957));
#13939=CARTESIAN_POINT('Ctrl Pts',(-109.647683916166,101.93405752606,-89.9278381616077));
#13940=CARTESIAN_POINT('Ctrl Pts',(-109.585780717548,102.121418154361,-90.0107041459795));
#13941=CARTESIAN_POINT('Ctrl Pts',(-109.399335228826,102.623158600648,-90.2043869062662));
#13942=CARTESIAN_POINT('Ctrl Pts',(-109.259387572093,102.942330744829,-90.2980516526588));
#13943=CARTESIAN_POINT('Ctrl Pts',(-108.856079275086,103.713602817721,-90.4495286319902));
#13944=CARTESIAN_POINT('Ctrl Pts',(-108.560802720886,104.170639304011,-90.4718337906789));
#13945=CARTESIAN_POINT('Ctrl Pts',(-107.984073142598,104.807412067022,-90.3754648931577));
#13946=CARTESIAN_POINT('Ctrl Pts',(-107.731615284225,105.031808587313,-90.3040840691712));
#13947=CARTESIAN_POINT('Ctrl Pts',(-107.274706570105,105.310186009746,-90.1276174249943));
#13948=CARTESIAN_POINT('Ctrl Pts',(-107.082643892882,105.395243156987,-90.0418124615454));
#13949=CARTESIAN_POINT('Ctrl Pts',(-106.81731713635,105.462525333909,-89.9082723306999));
#13950=CARTESIAN_POINT('Ctrl Pts',(-106.748607297535,105.475545269237,-89.8723672736483));
#13951=CARTESIAN_POINT('Ctrl Pts',(-106.617982888177,105.491574342406,-89.8015773906488));
#13952=CARTESIAN_POINT('Ctrl Pts',(-106.556276581001,105.495421682755,-89.7670559094086));
#13953=CARTESIAN_POINT('Ctrl Pts',(-106.49494062967,105.495421682755,-89.7316435813966));
#13954=CARTESIAN_POINT('Origin',(-119.078493020361,109.,-80.7499999999988));
#13955=CARTESIAN_POINT('Origin',(-98.8802009968175,127.881285087611,-122.304146684539));
#13956=CARTESIAN_POINT('',(-122.975807503838,96.7732359445554,-73.9996533015419));
#13957=CARTESIAN_POINT('Origin',(-102.225887894125,139.471084472322,-116.509246992184));
#13958=CARTESIAN_POINT('',(-126.321494401146,108.363035329266,-68.2047536091869));
#13959=CARTESIAN_POINT('Origin',(-91.1597915940262,130.212083164828,-116.292900852773));
#13960=CARTESIAN_POINT('',(-118.565048334243,98.5672184524784,-68.8256037842474));
#13961=CARTESIAN_POINT('',(-118.565048334243,98.5672184524783,-68.8256037842474));
#13962=CARTESIAN_POINT('',(-118.565048334243,98.5672184524784,-68.8256037842474));
#13963=CARTESIAN_POINT('Origin',(-93.159791594026,137.140286395103,-112.828799237635));
#13964=CARTESIAN_POINT('',(-120.565048334243,105.495421682754,-65.3615021691091));
#13965=CARTESIAN_POINT('',(-120.565048334243,105.495421682754,-65.3615021691091));
#13966=CARTESIAN_POINT('',(-120.565048334243,105.495421682754,-65.3615021691091));
#13967=CARTESIAN_POINT('Ctrl Pts',(-120.562281092551,105.498617018225,-65.3662951723163));
#13968=CARTESIAN_POINT('Ctrl Pts',(-121.122370810941,104.85188111886,-64.3961913232677));
#13969=CARTESIAN_POINT('Ctrl Pts',(-120.882918550091,105.498617018225,-65.5514152947396));
#13970=CARTESIAN_POINT('Ctrl Pts',(-121.443008268481,104.85188111886,-64.581311445691));
#13971=CARTESIAN_POINT('Ctrl Pts',(-121.471975862605,105.318247730476,-66.0117538845209));
#13972=CARTESIAN_POINT('Ctrl Pts',(-122.032065580995,104.67151183111,-65.0416500354723));
#13973=CARTESIAN_POINT('Ctrl Pts',(-122.064945259985,104.547775319114,-66.8677531999604));
#13974=CARTESIAN_POINT('Ctrl Pts',(-122.625034978375,103.901039419748,-65.8976493509118));
#13975=CARTESIAN_POINT('Ctrl Pts',(-122.276875185293,103.394681868295,-67.7588399665989));
#13976=CARTESIAN_POINT('Ctrl Pts',(-122.836964903683,102.747945968929,-66.7887361175503));
#13977=CARTESIAN_POINT('Ctrl Pts',(-122.075541779062,102.034515403088,-68.5493777137862));
#13978=CARTESIAN_POINT('Ctrl Pts',(-122.635631497452,101.387779503722,-67.5792738647376));
#13979=CARTESIAN_POINT('Ctrl Pts',(-121.491582710463,100.674348937881,-69.1190064318059));
#13980=CARTESIAN_POINT('Ctrl Pts',(-122.051672428853,100.027613038515,-68.1489025827573));
#13981=CARTESIAN_POINT('Ctrl Pts',(-120.613913970924,99.5212554870615,-69.3810131159864));
#13982=CARTESIAN_POINT('Ctrl Pts',(-121.174003689314,98.8745195876958,-68.4109092669378));
#13983=CARTESIAN_POINT('Ctrl Pts',(-119.576112119442,98.7507830756997,-69.2954862119089));
#13984=CARTESIAN_POINT('Ctrl Pts',(-120.136201837832,98.104047176334,-68.3253823628603));
#13985=CARTESIAN_POINT('Ctrl Pts',(-118.882918550091,98.5704137879498,-69.0155169098773));
#13986=CARTESIAN_POINT('Ctrl Pts',(-119.443008268481,97.9236778885841,-68.0454130608287));
#13987=CARTESIAN_POINT('Ctrl Pts',(-118.562281092551,98.5704137879498,-68.8303967874541));
#13988=CARTESIAN_POINT('Ctrl Pts',(-119.122370810941,97.9236778885841,-67.8602929384055));
#13989=CARTESIAN_POINT('Ctrl Pts',(-120.565048334243,105.495421682754,-65.3615021691091));
#13990=CARTESIAN_POINT('Ctrl Pts',(-120.691039416989,105.495421682754,-65.4342431546481));
#13991=CARTESIAN_POINT('Ctrl Pts',(-120.814135033437,105.479185279105,-65.509950975606));
#13992=CARTESIAN_POINT('Ctrl Pts',(-121.108798536521,105.401649043373,-65.7026970040038));
#13993=CARTESIAN_POINT('Ctrl Pts',(-121.272162868975,105.32340896221,-65.8200526993256));
#13994=CARTESIAN_POINT('Ctrl Pts',(-121.650625788444,105.059904053223,-66.1207099909364));
#13995=CARTESIAN_POINT('Ctrl Pts',(-121.841200031555,104.840955426175,-66.3026948775666));
#13996=CARTESIAN_POINT('Ctrl Pts',(-122.229702683097,104.20220248838,-66.7620575698267));
#13997=CARTESIAN_POINT('Ctrl Pts',(-122.365246282272,103.731292190713,-67.0375250373832));
#13998=CARTESIAN_POINT('Ctrl Pts',(-122.437834115624,102.945223269976,-67.4708463451536));
#13999=CARTESIAN_POINT('Ctrl Pts',(-122.426862867774,102.625337747109,-67.6392753478494));
#14000=CARTESIAN_POINT('Ctrl Pts',(-122.352414034946,102.122794062321,-67.8980171685339));
#14001=CARTESIAN_POINT('Ctrl Pts',(-122.311641017802,101.935332740824,-67.9931170741559));
#14002=CARTESIAN_POINT('Ctrl Pts',(-122.205060922126,101.565932484526,-68.1778231774862));
#14003=CARTESIAN_POINT('Ctrl Pts',(-122.139064926783,101.383297810808,-68.2677780937319));
#14004=CARTESIAN_POINT('Ctrl Pts',(-121.931077153049,100.906432252622,-68.4987731861706));
#14005=CARTESIAN_POINT('Ctrl Pts',(-121.766241312432,100.615998507772,-68.6355455315589));
#14006=CARTESIAN_POINT('Ctrl Pts',(-121.278590206767,99.9421171214444,-68.9331085407376));
#14007=CARTESIAN_POINT('Ctrl Pts',(-120.910627382145,99.5690115107432,-69.0813100128094));
#14008=CARTESIAN_POINT('Ctrl Pts',(-120.211847266071,99.0731705694225,-69.1963388478251));
#14009=CARTESIAN_POINT('Ctrl Pts',(-119.910531355856,98.9051904678996,-69.2095826519892));
#14010=CARTESIAN_POINT('Ctrl Pts',(-119.389804002114,98.7005044629965,-69.1436531341076));
#14011=CARTESIAN_POINT('Ctrl Pts',(-119.177202045119,98.6391640331656,-69.0934232467741));
#14012=CARTESIAN_POINT('Ctrl Pts',(-118.895501925765,98.5907881871084,-68.988242612226));
#14013=CARTESIAN_POINT('Ctrl Pts',(-118.823599460482,98.5814547792815,-68.9578673464248));
#14014=CARTESIAN_POINT('Ctrl Pts',(-118.689039034596,98.5699706265173,-68.8938948440334));
#14015=CARTESIAN_POINT('Ctrl Pts',(-118.626384285574,98.5672184524785,-68.8610161122592));
#14016=CARTESIAN_POINT('Ctrl Pts',(-118.565048334243,98.5672184524785,-68.8256037842472));
#14017=CARTESIAN_POINT('Origin',(-119.078493020361,109.,-80.7499999999988));
#14018=CARTESIAN_POINT('Origin',(-69.3034604663987,124.991664350565,-51.4350212868557));
#14019=CARTESIAN_POINT('',(-67.366968793295,124.991664350565,-50.3169872981059));
#14020=CARTESIAN_POINT('Origin',(-68.8034604663987,123.191664350565,-52.3010466906402));
#14021=CARTESIAN_POINT('',(-66.866968793295,124.991664350565,-51.1830127018903));
#14022=CARTESIAN_POINT('Origin',(-69.3034604663987,124.991664350565,-51.4350212868557));
#14023=CARTESIAN_POINT('Origin',(-76.346812504256,100.571155122824,-40.3758635351318));
#14024=CARTESIAN_POINT('',(-73.9165625814855,100.571155122824,-38.9727580880221));
#14025=CARTESIAN_POINT('Origin',(-75.81738964085,102.337180526609,-41.2928508332395));
#14026=CARTESIAN_POINT('',(-74.1665625814855,101.437180526609,-38.5397453861299));
#14027=CARTESIAN_POINT('Origin',(-76.346812504256,100.571155122824,-40.3758635351318));
#14028=CARTESIAN_POINT('Origin',(-62.497624927873,101.437180526611,-64.3633600609793));
#14029=CARTESIAN_POINT('',(-60.0673750051025,101.437180526611,-62.9602546138697));
#14030=CARTESIAN_POINT('Origin',(-63.527047791279,101.471155122826,-62.580347359087));
#14031=CARTESIAN_POINT('',(-60.3173750051025,100.571155122826,-62.5272419119774));
#14032=CARTESIAN_POINT('Origin',(-62.497624927873,101.437180526611,-64.3633600609793));
#14033=CARTESIAN_POINT('',(-0.662546388783154,39.9624663095064,11.3449915063472));
#14034=CARTESIAN_POINT('',(-12.7683873876991,56.3012899998748,43.4781798467456));
#14035=CARTESIAN_POINT('',(-22.4000040844042,254.577374315256,38.728643251025));
#14036=CARTESIAN_POINT('',(-44.7393996466421,286.888929591391,-0.542249927592924));
#14037=CARTESIAN_POINT('',(-75.4310082996939,297.414432149061,-39.0811659930832));
#14038=CARTESIAN_POINT('',(-10.0317249986676,270.739548408369,-15.7797463643511));
#14039=CARTESIAN_POINT('',(-22.6769527544393,36.8799811186442,39.4637630808387));
#14040=CARTESIAN_POINT('',(43.9283203292622,145.048364335116,-137.330214690215));
#14041=CARTESIAN_POINT('',(-70.150751068712,45.7295323022975,66.908474173488));
#14042=CARTESIAN_POINT('',(16.1850811205472,103.887257875328,-162.257393485845));
#14043=CARTESIAN_POINT('',(-117.405702678433,62.3288247714053,72.3345349171988));
#14044=CARTESIAN_POINT('',(-24.6426326618715,76.7624628485525,-173.891497635406));
#14045=CARTESIAN_POINT('',(-44.5237921714637,76.7498579606653,75.7744125587609));
#14046=CARTESIAN_POINT('',(31.9506663628748,89.0163133999874,-127.215877792275));
#14047=CARTESIAN_POINT('',(87.7528075856479,118.446581197511,72.166262746054));
#14048=CARTESIAN_POINT('',(-114.336680224609,122.155176814109,18.5067544696373));
#14049=CARTESIAN_POINT('',(156.852261979979,102.394343099889,49.8243091599253));
#14050=CARTESIAN_POINT('',(-128.302481149164,126.980744084233,91.3987440201974));
#14051=CARTESIAN_POINT('',(125.207758354551,135.554210316916,70.7302340080619));
#14052=CARTESIAN_POINT('',(-132.467824017269,147.415774201419,45.5395185556597));
#14053=CARTESIAN_POINT('',(87.7903907288698,176.604712884864,70.4385348843062));
#14054=CARTESIAN_POINT('',(-115.780935769008,178.014605066633,2.28969127545628));
#14055=CARTESIAN_POINT('',(-28.0527374746009,17.2091314444563,-90.0766520029799));
#14056=CARTESIAN_POINT('',(88.7995497444537,29.0706953289587,25.8320712588734));
#14057=CARTESIAN_POINT('',(-27.2614083722717,24.866918647796,-35.0673769405371));
#14058=CARTESIAN_POINT('',(40.2866580643077,26.276810829564,-1.07483862929082));
#14059=CARTESIAN_POINT('',(-10.2344416225568,21.1192365738832,-137.036512608739));
#14060=CARTESIAN_POINT('',(120.545250077718,45.7056375582261,61.2368492512013));
#14061=CARTESIAN_POINT('',(-49.9760505799272,51.092210612468,-81.7753401605953));
#14062=CARTESIAN_POINT('',(90.7300551805382,54.8008062290654,-6.29021121846456));
#14063=CARTESIAN_POINT('',(5.78878308239131,265.950032180892,-108.404435581786));
#14064=CARTESIAN_POINT('',(75.4636454975784,277.811596065395,-10.2693112969086));
#14065=CARTESIAN_POINT('',(-37.7091798762756,232.919249963707,-98.2958800933581));
#14066=CARTESIAN_POINT('',(89.8572173262556,234.329142145475,-41.6920664372532));
#14067=CARTESIAN_POINT('',(53.8763942611725,276.112538618732,-119.464011130862));
#14068=CARTESIAN_POINT('',(60.7764656851507,300.698939603075,32.1390057205366));
#14069=CARTESIAN_POINT('',(2.66523287748433,261.404034534145,-67.5732731046087));
#14070=CARTESIAN_POINT('',(41.8035915604113,265.112630150743,-30.352725433204));
#14071=CARTESIAN_POINT('',(-36.6204283408977,44.9494746311851,-34.3043968237705));
#14072=CARTESIAN_POINT('',(43.2414227609921,43.1448698330196,-15.1539152787323));
#14073=CARTESIAN_POINT('',(0.,0.,0.));
#14074=CARTESIAN_POINT('Origin',(0.,89.,-11.9999999999999));
#14075=CARTESIAN_POINT('',(-1.95943487863577E-15,89.,4.00000000000008));
#14076=CARTESIAN_POINT('Origin',(0.,89.,-11.9999999999999));
#14077=CARTESIAN_POINT('',(-1.93805207434485E-15,94.,3.82539615254134));
#14078=CARTESIAN_POINT('',(-1.95943487863577E-15,89.,4.00000000000008));
#14079=CARTESIAN_POINT('Origin',(0.,94.,-11.9999999999999));
#14080=CARTESIAN_POINT('Origin',(0.,94.,-11.9999999999999));
#14081=CARTESIAN_POINT('',(-1.46957615897682E-15,94.,8.21565038222616E-14));
#14082=CARTESIAN_POINT('Origin',(0.,94.,-11.9999999999999));
#14083=CARTESIAN_POINT('Origin',(0.,89.,-11.9999999999999));
#14084=CARTESIAN_POINT('',(0.,89.,-25.9999999999999));
#14085=CARTESIAN_POINT('Origin',(0.,89.,-11.9999999999999));
#14086=CARTESIAN_POINT('Origin',(0.,79.,-11.9999999999999));
#14087=CARTESIAN_POINT('',(0.,79.,-25.9999999999999));
#14088=CARTESIAN_POINT('',(-1.71450551880629E-15,79.,-25.9999999999999));
#14089=CARTESIAN_POINT('Origin',(0.,79.,-11.9999999999999));
#14090=CARTESIAN_POINT('Origin',(0.,79.,-11.9999999999999));
#14091=CARTESIAN_POINT('',(-1.46957615897682E-15,79.,8.21565038222616E-14));
#14092=CARTESIAN_POINT('Origin',(0.,79.,-11.9999999999999));
#14093=CARTESIAN_POINT('Origin',(0.,136.,-11.9999999999999));
#14094=CARTESIAN_POINT('',(-1.46957615897682E-15,136.,8.21565038222616E-14));
#14095=CARTESIAN_POINT('',(0.,0.,11.9999999999999));
#14096=CARTESIAN_POINT('',(0.,0.,11.9999999999999));
#14097=CARTESIAN_POINT('',(-78.3247785391372,-1.19157009728788,3.52582637351323));
#14098=CARTESIAN_POINT('',(-7.49431551401068,-37.4712389911551,1.73467830808887));
#14099=CARTESIAN_POINT('',(6.55216660792492,0.,-10.053313520526));
#14100=UNCERTAINTY_MEASURE_WITH_UNIT(LENGTH_MEASURE(0.01),#14126,
'DISTANCE_ACCURACY_VALUE',
'Maximum model space distance between geometric entities at asserted c
onnectivities');
#14101=UNCERTAINTY_MEASURE_WITH_UNIT(LENGTH_MEASURE(0.01),#14126,
'DISTANCE_ACCURACY_VALUE',
'Maximum model space distance between geometric entities at asserted c
onnectivities');
#14102=UNCERTAINTY_MEASURE_WITH_UNIT(LENGTH_MEASURE(0.01),#14126,
'DISTANCE_ACCURACY_VALUE',
'Maximum model space distance between geometric entities at asserted c
onnectivities');
#14103=UNCERTAINTY_MEASURE_WITH_UNIT(LENGTH_MEASURE(0.01),#14126,
'DISTANCE_ACCURACY_VALUE',
'Maximum model space distance between geometric entities at asserted c
onnectivities');
#14104=UNCERTAINTY_MEASURE_WITH_UNIT(LENGTH_MEASURE(0.01),#14126,
'DISTANCE_ACCURACY_VALUE',
'Maximum model space distance between geometric entities at asserted c
onnectivities');
#14105=UNCERTAINTY_MEASURE_WITH_UNIT(LENGTH_MEASURE(0.01),#14126,
'DISTANCE_ACCURACY_VALUE',
'Maximum model space distance between geometric entities at asserted c
onnectivities');
#14106=UNCERTAINTY_MEASURE_WITH_UNIT(LENGTH_MEASURE(0.01),#14126,
'DISTANCE_ACCURACY_VALUE',
'Maximum model space distance between geometric entities at asserted c
onnectivities');
#14107=UNCERTAINTY_MEASURE_WITH_UNIT(LENGTH_MEASURE(0.01),#14126,
'DISTANCE_ACCURACY_VALUE',
'Maximum model space distance between geometric entities at asserted c
onnectivities');
#14108=UNCERTAINTY_MEASURE_WITH_UNIT(LENGTH_MEASURE(0.01),#14126,
'DISTANCE_ACCURACY_VALUE',
'Maximum model space distance between geometric entities at asserted c
onnectivities');
#14109=UNCERTAINTY_MEASURE_WITH_UNIT(LENGTH_MEASURE(0.01),#14126,
'DISTANCE_ACCURACY_VALUE',
'Maximum model space distance between geometric entities at asserted c
onnectivities');
#14110=UNCERTAINTY_MEASURE_WITH_UNIT(LENGTH_MEASURE(0.01),#14126,
'DISTANCE_ACCURACY_VALUE',
'Maximum model space distance between geometric entities at asserted c
onnectivities');
#14111=UNCERTAINTY_MEASURE_WITH_UNIT(LENGTH_MEASURE(0.01),#14126,
'DISTANCE_ACCURACY_VALUE',
'Maximum model space distance between geometric entities at asserted c
onnectivities');
#14112=UNCERTAINTY_MEASURE_WITH_UNIT(LENGTH_MEASURE(0.01),#14126,
'DISTANCE_ACCURACY_VALUE',
'Maximum model space distance between geometric entities at asserted c
onnectivities');
#14113=(
GEOMETRIC_REPRESENTATION_CONTEXT(3)
GLOBAL_UNCERTAINTY_ASSIGNED_CONTEXT((#14100))
GLOBAL_UNIT_ASSIGNED_CONTEXT((#14126,#14128,#14129))
REPRESENTATION_CONTEXT('','3D')
);
#14114=(
GEOMETRIC_REPRESENTATION_CONTEXT(3)
GLOBAL_UNCERTAINTY_ASSIGNED_CONTEXT((#14101))
GLOBAL_UNIT_ASSIGNED_CONTEXT((#14126,#14128,#14129))
REPRESENTATION_CONTEXT('','3D')
);
#14115=(
GEOMETRIC_REPRESENTATION_CONTEXT(3)
GLOBAL_UNCERTAINTY_ASSIGNED_CONTEXT((#14102))
GLOBAL_UNIT_ASSIGNED_CONTEXT((#14126,#14128,#14129))
REPRESENTATION_CONTEXT('','3D')
);
#14116=(
GEOMETRIC_REPRESENTATION_CONTEXT(3)
GLOBAL_UNCERTAINTY_ASSIGNED_CONTEXT((#14103))
GLOBAL_UNIT_ASSIGNED_CONTEXT((#14126,#14128,#14129))
REPRESENTATION_CONTEXT('','3D')
);
#14117=(
GEOMETRIC_REPRESENTATION_CONTEXT(3)
GLOBAL_UNCERTAINTY_ASSIGNED_CONTEXT((#14104))
GLOBAL_UNIT_ASSIGNED_CONTEXT((#14126,#14128,#14129))
REPRESENTATION_CONTEXT('','3D')
);
#14118=(
GEOMETRIC_REPRESENTATION_CONTEXT(3)
GLOBAL_UNCERTAINTY_ASSIGNED_CONTEXT((#14105))
GLOBAL_UNIT_ASSIGNED_CONTEXT((#14126,#14128,#14129))
REPRESENTATION_CONTEXT('','3D')
);
#14119=(
GEOMETRIC_REPRESENTATION_CONTEXT(3)
GLOBAL_UNCERTAINTY_ASSIGNED_CONTEXT((#14106))
GLOBAL_UNIT_ASSIGNED_CONTEXT((#14126,#14128,#14129))
REPRESENTATION_CONTEXT('','3D')
);
#14120=(
GEOMETRIC_REPRESENTATION_CONTEXT(3)
GLOBAL_UNCERTAINTY_ASSIGNED_CONTEXT((#14107))
GLOBAL_UNIT_ASSIGNED_CONTEXT((#14126,#14128,#14129))
REPRESENTATION_CONTEXT('','3D')
);
#14121=(
GEOMETRIC_REPRESENTATION_CONTEXT(3)
GLOBAL_UNCERTAINTY_ASSIGNED_CONTEXT((#14108))
GLOBAL_UNIT_ASSIGNED_CONTEXT((#14126,#14128,#14129))
REPRESENTATION_CONTEXT('','3D')
);
#14122=(
GEOMETRIC_REPRESENTATION_CONTEXT(3)
GLOBAL_UNCERTAINTY_ASSIGNED_CONTEXT((#14109))
GLOBAL_UNIT_ASSIGNED_CONTEXT((#14126,#14128,#14129))
REPRESENTATION_CONTEXT('','3D')
);
#14123=(
GEOMETRIC_REPRESENTATION_CONTEXT(3)
GLOBAL_UNCERTAINTY_ASSIGNED_CONTEXT((#14110))
GLOBAL_UNIT_ASSIGNED_CONTEXT((#14126,#14128,#14129))
REPRESENTATION_CONTEXT('','3D')
);
#14124=(
GEOMETRIC_REPRESENTATION_CONTEXT(3)
GLOBAL_UNCERTAINTY_ASSIGNED_CONTEXT((#14111))
GLOBAL_UNIT_ASSIGNED_CONTEXT((#14126,#14128,#14129))
REPRESENTATION_CONTEXT('','3D')
);
#14125=(
GEOMETRIC_REPRESENTATION_CONTEXT(3)
GLOBAL_UNCERTAINTY_ASSIGNED_CONTEXT((#14112))
GLOBAL_UNIT_ASSIGNED_CONTEXT((#14126,#14128,#14129))
REPRESENTATION_CONTEXT('','3D')
);
#14126=(
LENGTH_UNIT()
NAMED_UNIT(*)
SI_UNIT(.MILLI.,.METRE.)
);
#14127=(
LENGTH_UNIT()
NAMED_UNIT(*)
SI_UNIT($,.METRE.)
);
#14128=(
NAMED_UNIT(*)
PLANE_ANGLE_UNIT()
SI_UNIT($,.RADIAN.)
);
#14129=(
NAMED_UNIT(*)
SI_UNIT($,.STERADIAN.)
SOLID_ANGLE_UNIT()
);
#14130=SHAPE_DEFINITION_REPRESENTATION(#14142,#14199);
#14131=SHAPE_DEFINITION_REPRESENTATION(#14143,#14200);
#14132=SHAPE_DEFINITION_REPRESENTATION(#14144,#14201);
#14133=SHAPE_DEFINITION_REPRESENTATION(#14145,#14202);
#14134=SHAPE_DEFINITION_REPRESENTATION(#14146,#14203);
#14135=SHAPE_DEFINITION_REPRESENTATION(#14147,#14204);
#14136=SHAPE_DEFINITION_REPRESENTATION(#14148,#14205);
#14137=SHAPE_DEFINITION_REPRESENTATION(#14149,#14206);
#14138=SHAPE_DEFINITION_REPRESENTATION(#14150,#14207);
#14139=SHAPE_DEFINITION_REPRESENTATION(#14151,#14208);
#14140=SHAPE_DEFINITION_REPRESENTATION(#14152,#14209);
#14141=SHAPE_DEFINITION_REPRESENTATION(#14193,#14210);
#14142=PRODUCT_DEFINITION_SHAPE('',$,#14212);
#14143=PRODUCT_DEFINITION_SHAPE('',$,#14213);
#14144=PRODUCT_DEFINITION_SHAPE('',$,#14214);
#14145=PRODUCT_DEFINITION_SHAPE('',$,#14215);
#14146=PRODUCT_DEFINITION_SHAPE('',$,#14216);
#14147=PRODUCT_DEFINITION_SHAPE('',$,#14217);
#14148=PRODUCT_DEFINITION_SHAPE('',$,#14218);
#14149=PRODUCT_DEFINITION_SHAPE('',$,#14219);
#14150=PRODUCT_DEFINITION_SHAPE('',$,#14220);
#14151=PRODUCT_DEFINITION_SHAPE('',$,#14221);
#14152=PRODUCT_DEFINITION_SHAPE('',$,#14222);
#14153=PRODUCT_DEFINITION_SHAPE($,$,#146);
#14154=PRODUCT_DEFINITION_SHAPE($,$,#147);
#14155=PRODUCT_DEFINITION_SHAPE($,$,#148);
#14156=PRODUCT_DEFINITION_SHAPE($,$,#149);
#14157=PRODUCT_DEFINITION_SHAPE($,$,#150);
#14158=PRODUCT_DEFINITION_SHAPE($,$,#151);
#14159=PRODUCT_DEFINITION_SHAPE($,$,#152);
#14160=PRODUCT_DEFINITION_SHAPE($,$,#153);
#14161=PRODUCT_DEFINITION_SHAPE($,$,#154);
#14162=PRODUCT_DEFINITION_SHAPE($,$,#155);
#14163=PRODUCT_DEFINITION_SHAPE($,$,#156);
#14164=PRODUCT_DEFINITION_SHAPE($,$,#157);
#14165=PRODUCT_DEFINITION_SHAPE($,$,#158);
#14166=PRODUCT_DEFINITION_SHAPE($,$,#159);
#14167=PRODUCT_DEFINITION_SHAPE($,$,#160);
#14168=PRODUCT_DEFINITION_SHAPE($,$,#161);
#14169=PRODUCT_DEFINITION_SHAPE($,$,#162);
#14170=PRODUCT_DEFINITION_SHAPE($,$,#163);
#14171=PRODUCT_DEFINITION_SHAPE($,$,#164);
#14172=PRODUCT_DEFINITION_SHAPE($,$,#165);
#14173=PRODUCT_DEFINITION_SHAPE($,$,#166);
#14174=PRODUCT_DEFINITION_SHAPE($,$,#167);
#14175=PRODUCT_DEFINITION_SHAPE($,$,#168);
#14176=PRODUCT_DEFINITION_SHAPE($,$,#169);
#14177=PRODUCT_DEFINITION_SHAPE($,$,#170);
#14178=PRODUCT_DEFINITION_SHAPE($,$,#171);
#14179=PRODUCT_DEFINITION_SHAPE($,$,#172);
#14180=PRODUCT_DEFINITION_SHAPE($,$,#173);
#14181=PRODUCT_DEFINITION_SHAPE($,$,#174);
#14182=PRODUCT_DEFINITION_SHAPE($,$,#175);
#14183=PRODUCT_DEFINITION_SHAPE($,$,#176);
#14184=PRODUCT_DEFINITION_SHAPE($,$,#177);
#14185=PRODUCT_DEFINITION_SHAPE($,$,#178);
#14186=PRODUCT_DEFINITION_SHAPE($,$,#179);
#14187=PRODUCT_DEFINITION_SHAPE($,$,#180);
#14188=PRODUCT_DEFINITION_SHAPE($,$,#181);
#14189=PRODUCT_DEFINITION_SHAPE($,$,#182);
#14190=PRODUCT_DEFINITION_SHAPE($,$,#183);
#14191=PRODUCT_DEFINITION_SHAPE($,$,#184);
#14192=PRODUCT_DEFINITION_SHAPE($,$,#185);
#14193=PRODUCT_DEFINITION_SHAPE('',$,#14223);
#14194=PRODUCT_DEFINITION_SHAPE($,$,#186);
#14195=PRODUCT_DEFINITION_SHAPE($,$,#187);
#14196=PRODUCT_DEFINITION_SHAPE($,$,#188);
#14197=PRODUCT_DEFINITION_SHAPE($,$,#189);
#14198=PRODUCT_DEFINITION_SHAPE($,$,#190);
#14199=SHAPE_REPRESENTATION('',(#6258,#6902,#6903,#6904,#6905,#6906),#14113);
#14200=SHAPE_REPRESENTATION('',(#6259),#14114);
#14201=SHAPE_REPRESENTATION('',(#6338),#14115);
#14202=SHAPE_REPRESENTATION('',(#6408),#14116);
#14203=SHAPE_REPRESENTATION('',(#6477,#6849,#6850,#6851,#6852,#6853,#6854,
#6855,#6856,#6857,#6858,#6859,#6860,#6861,#6862,#6863,#6864,#6865,#6866,
#6867,#6868,#6869,#6870,#6871,#6872,#6873,#6874,#6875,#6876,#6877,#6878,
#6879,#6880,#6881,#6882,#6883,#6884,#6885,#6886,#6887,#6888),#14117);
#14204=SHAPE_REPRESENTATION('',(#6478),#14118);
#14205=SHAPE_REPRESENTATION('',(#6609),#14119);
#14206=SHAPE_REPRESENTATION('',(#6624),#14120);
#14207=SHAPE_REPRESENTATION('',(#6639),#14121);
#14208=SHAPE_REPRESENTATION('',(#6654),#14122);
#14209=SHAPE_REPRESENTATION('',(#6669),#14123);
#14210=SHAPE_REPRESENTATION('',(#6889),#14124);
#14211=PRODUCT_DEFINITION_CONTEXT('part definition',#14249,'design');
#14212=PRODUCT_DEFINITION('MAT-062','MAT-062',#14224,
#14211);
#14213=PRODUCT_DEFINITION('Base Plate','Base Plate',#14225,#14211);
#14214=PRODUCT_DEFINITION('Back Lid','Back Lid',#14226,#14211);
#14215=PRODUCT_DEFINITION('Front Tightener','Front Tightener',#14227,#14211);
#14216=PRODUCT_DEFINITION('Rotating Assembly','Rotating Assembly',#14228,
#14211);
#14217=PRODUCT_DEFINITION('Top','Top',#14229,#14211);
#14218=PRODUCT_DEFINITION('Nozzle 60','Nozzle 60',#14230,#14211);
#14219=PRODUCT_DEFINITION('Nozzle 45','Nozzle 45',#14231,#14211);
#14220=PRODUCT_DEFINITION('Nozzle 75','Nozzle 75',#14232,#14211);
#14221=PRODUCT_DEFINITION('Nozzle 90','Nozzle 90',#14233,#14211);
#14222=PRODUCT_DEFINITION('Sprinkler','Sprinkler',#14234,#14211);
#14223=PRODUCT_DEFINITION('Connector','Connector',#14235,#14211);
#14224=PRODUCT_DEFINITION_FORMATION('',$,#14251);
#14225=PRODUCT_DEFINITION_FORMATION('',$,#14252);
#14226=PRODUCT_DEFINITION_FORMATION('',$,#14253);
#14227=PRODUCT_DEFINITION_FORMATION('',$,#14254);
#14228=PRODUCT_DEFINITION_FORMATION('',$,#14255);
#14229=PRODUCT_DEFINITION_FORMATION('',$,#14256);
#14230=PRODUCT_DEFINITION_FORMATION('',$,#14257);
#14231=PRODUCT_DEFINITION_FORMATION('',$,#14258);
#14232=PRODUCT_DEFINITION_FORMATION('',$,#14259);
#14233=PRODUCT_DEFINITION_FORMATION('',$,#14260);
#14234=PRODUCT_DEFINITION_FORMATION('',$,#14261);
#14235=PRODUCT_DEFINITION_FORMATION('',$,#14262);
#14236=PRODUCT_RELATED_PRODUCT_CATEGORY('MAT-062',
'MAT-062',(#14251));
#14237=PRODUCT_RELATED_PRODUCT_CATEGORY('Base Plate','Base Plate',(#14252));
#14238=PRODUCT_RELATED_PRODUCT_CATEGORY('Back Lid','Back Lid',(#14253));
#14239=PRODUCT_RELATED_PRODUCT_CATEGORY('Front Tightener',
'Front Tightener',(#14254));
#14240=PRODUCT_RELATED_PRODUCT_CATEGORY('Rotating Assembly',
'Rotating Assembly',(#14255));
#14241=PRODUCT_RELATED_PRODUCT_CATEGORY('Top','Top',(#14256));
#14242=PRODUCT_RELATED_PRODUCT_CATEGORY('Nozzle 60','Nozzle 60',(#14257));
#14243=PRODUCT_RELATED_PRODUCT_CATEGORY('Nozzle 45','Nozzle 45',(#14258));
#14244=PRODUCT_RELATED_PRODUCT_CATEGORY('Nozzle 75','Nozzle 75',(#14259));
#14245=PRODUCT_RELATED_PRODUCT_CATEGORY('Nozzle 90','Nozzle 90',(#14260));
#14246=PRODUCT_RELATED_PRODUCT_CATEGORY('Sprinkler','Sprinkler',(#14261));
#14247=PRODUCT_RELATED_PRODUCT_CATEGORY('Connector','Connector',(#14262));
#14248=APPLICATION_PROTOCOL_DEFINITION('international standard',
'automotive_design',2009,#14249);
#14249=APPLICATION_CONTEXT(
'Core Data for Automotive Mechanical Design Process');
#14250=PRODUCT_CONTEXT('part definition',#14249,'mechanical');
#14251=PRODUCT('MAT-062','MAT-062',
'LEGAL AND USAGE DISCLAIMER: this Data/Model is provided \X2\201C\X0\A
S IS\X2\201D\X0\ for informational and representational only. It is a 
geometric approximation and is NOT engineered, certified, or guarantee
d for dimensional accuracy, exact tolerances, or production-level prec
ision. Vendor disclaims all implied warranties including fitness for a
 particular purpose. DO NOT USE FOR DIRECT PHYSICAL MANUFACTURING, AUT
OMATED PRODUCTION, OR SAFETY-CRITICAL SYSTEMS without independent engi
neering verification and resolution of any design discrepancies.',(#14250));
#14252=PRODUCT('Base Plate','Base Plate',$,(#14250));
#14253=PRODUCT('Back Lid','Back Lid',$,(#14250));
#14254=PRODUCT('Front Tightener','Front Tightener',$,(#14250));
#14255=PRODUCT('Rotating Assembly','Rotating Assembly',$,(#14250));
#14256=PRODUCT('Top','Top',$,(#14250));
#14257=PRODUCT('Nozzle 60','Nozzle 60',$,(#14250));
#14258=PRODUCT('Nozzle 45','Nozzle 45',$,(#14250));
#14259=PRODUCT('Nozzle 75','Nozzle 75',$,(#14250));
#14260=PRODUCT('Nozzle 90','Nozzle 90',$,(#14250));
#14261=PRODUCT('Sprinkler','Sprinkler',$,(#14250));
#14262=PRODUCT('Connector','Connector',$,(#14250));
#14263=PRESENTATION_STYLE_ASSIGNMENT((#14265));
#14264=PRESENTATION_STYLE_ASSIGNMENT((#14266));
#14265=SURFACE_STYLE_USAGE(.BOTH.,#14267);
#14266=SURFACE_STYLE_USAGE(.BOTH.,#14268);
#14267=SURFACE_SIDE_STYLE('',(#14269));
#14268=SURFACE_SIDE_STYLE('',(#14270));
#14269=SURFACE_STYLE_FILL_AREA(#14271);
#14270=SURFACE_STYLE_FILL_AREA(#14272);
#14271=FILL_AREA_STYLE('Steel - Satin',(#14273));
#14272=FILL_AREA_STYLE('Opaque(255,255,255)',(#14274));
#14273=FILL_AREA_STYLE_COLOUR('Steel - Satin',#14275);
#14274=FILL_AREA_STYLE_COLOUR('Opaque(255,255,255)',#14276);
#14275=COLOUR_RGB('Steel - Satin',0.627450980392157,0.627450980392157,0.627450980392157);
#14276=COLOUR_RGB('Opaque(255,255,255)',1.,1.,1.);
ENDSEC;
END-ISO-10303-21;
